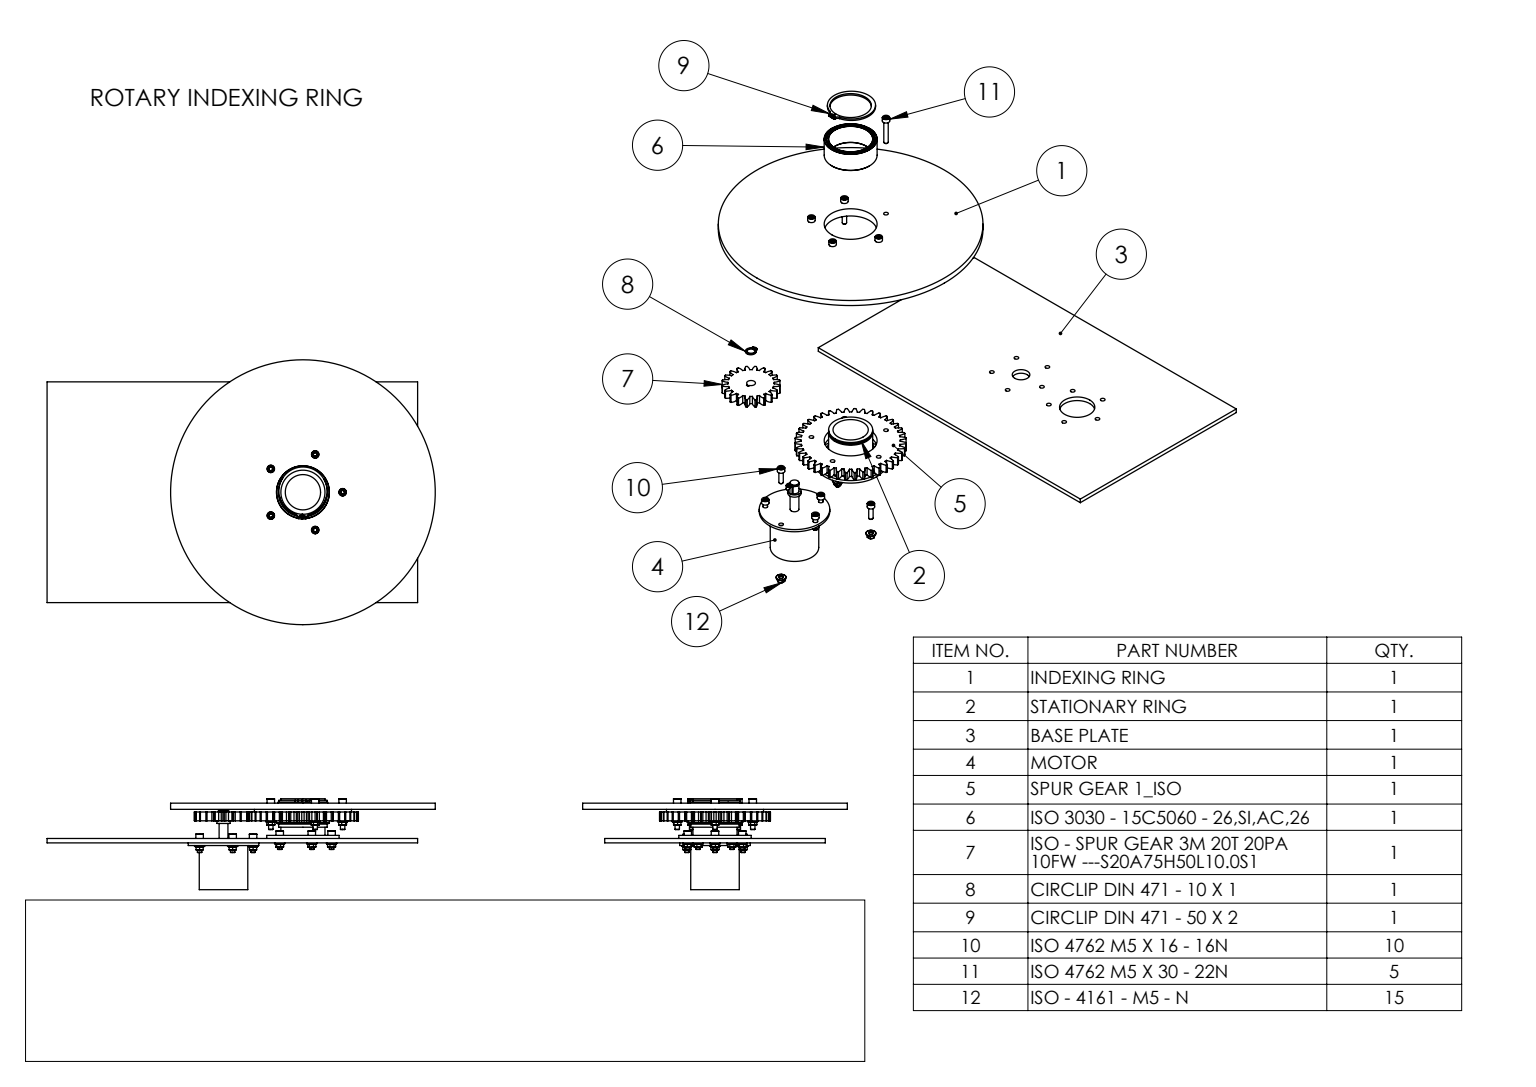
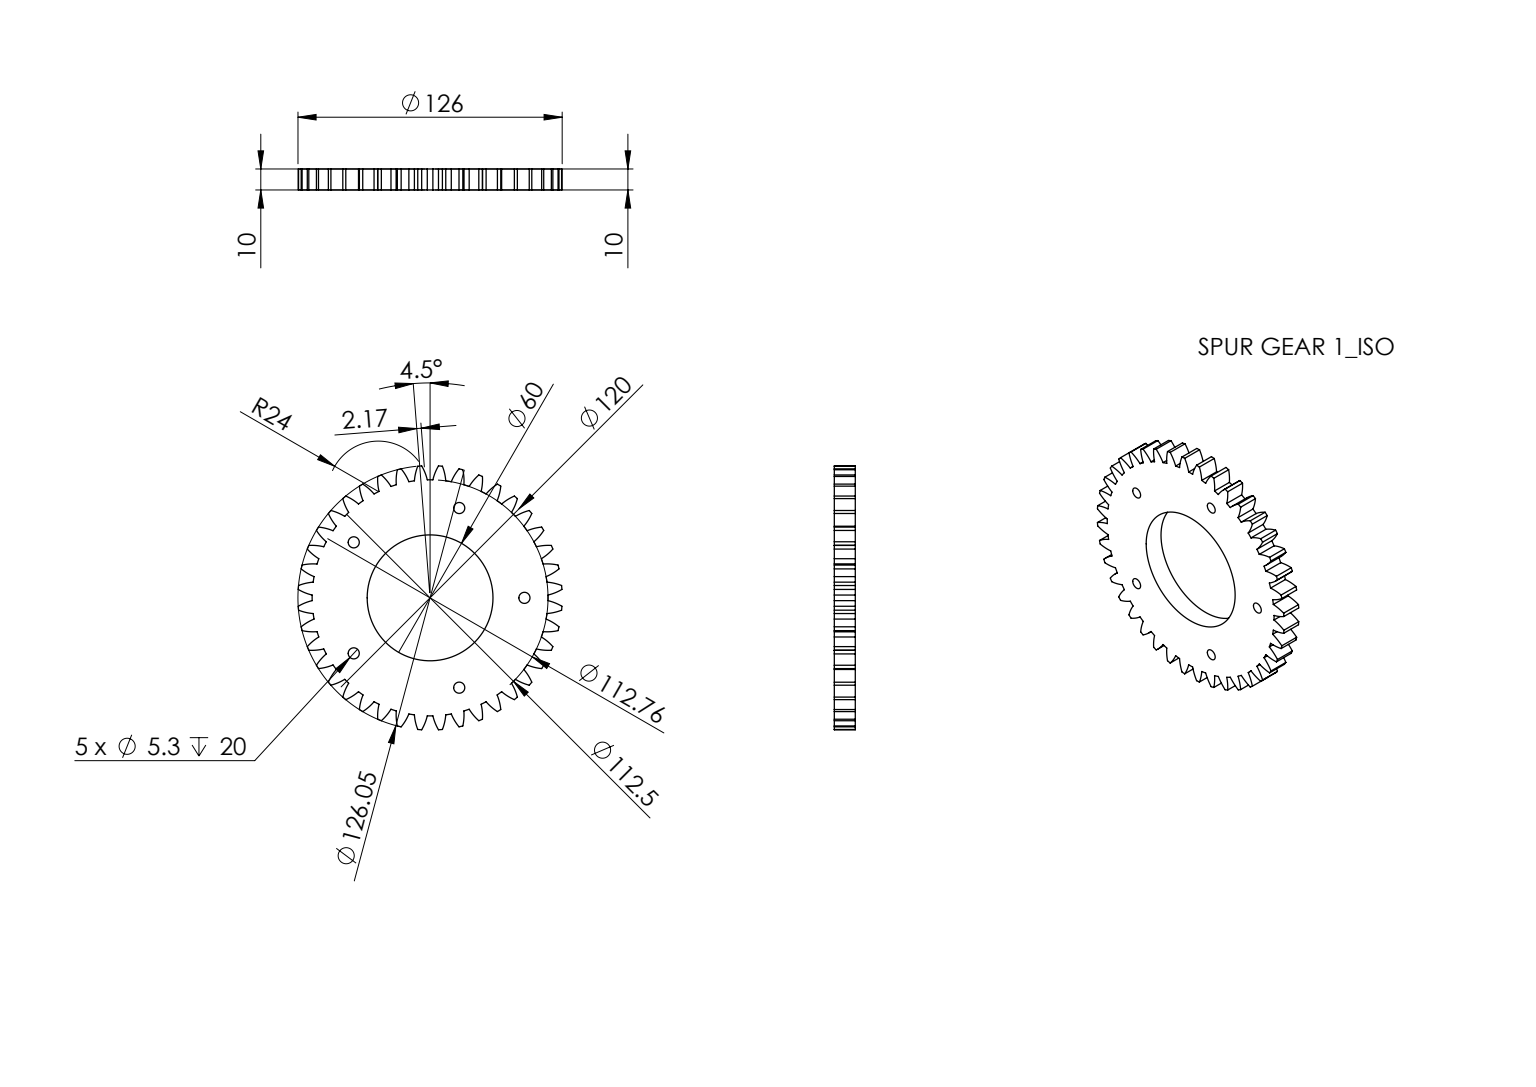
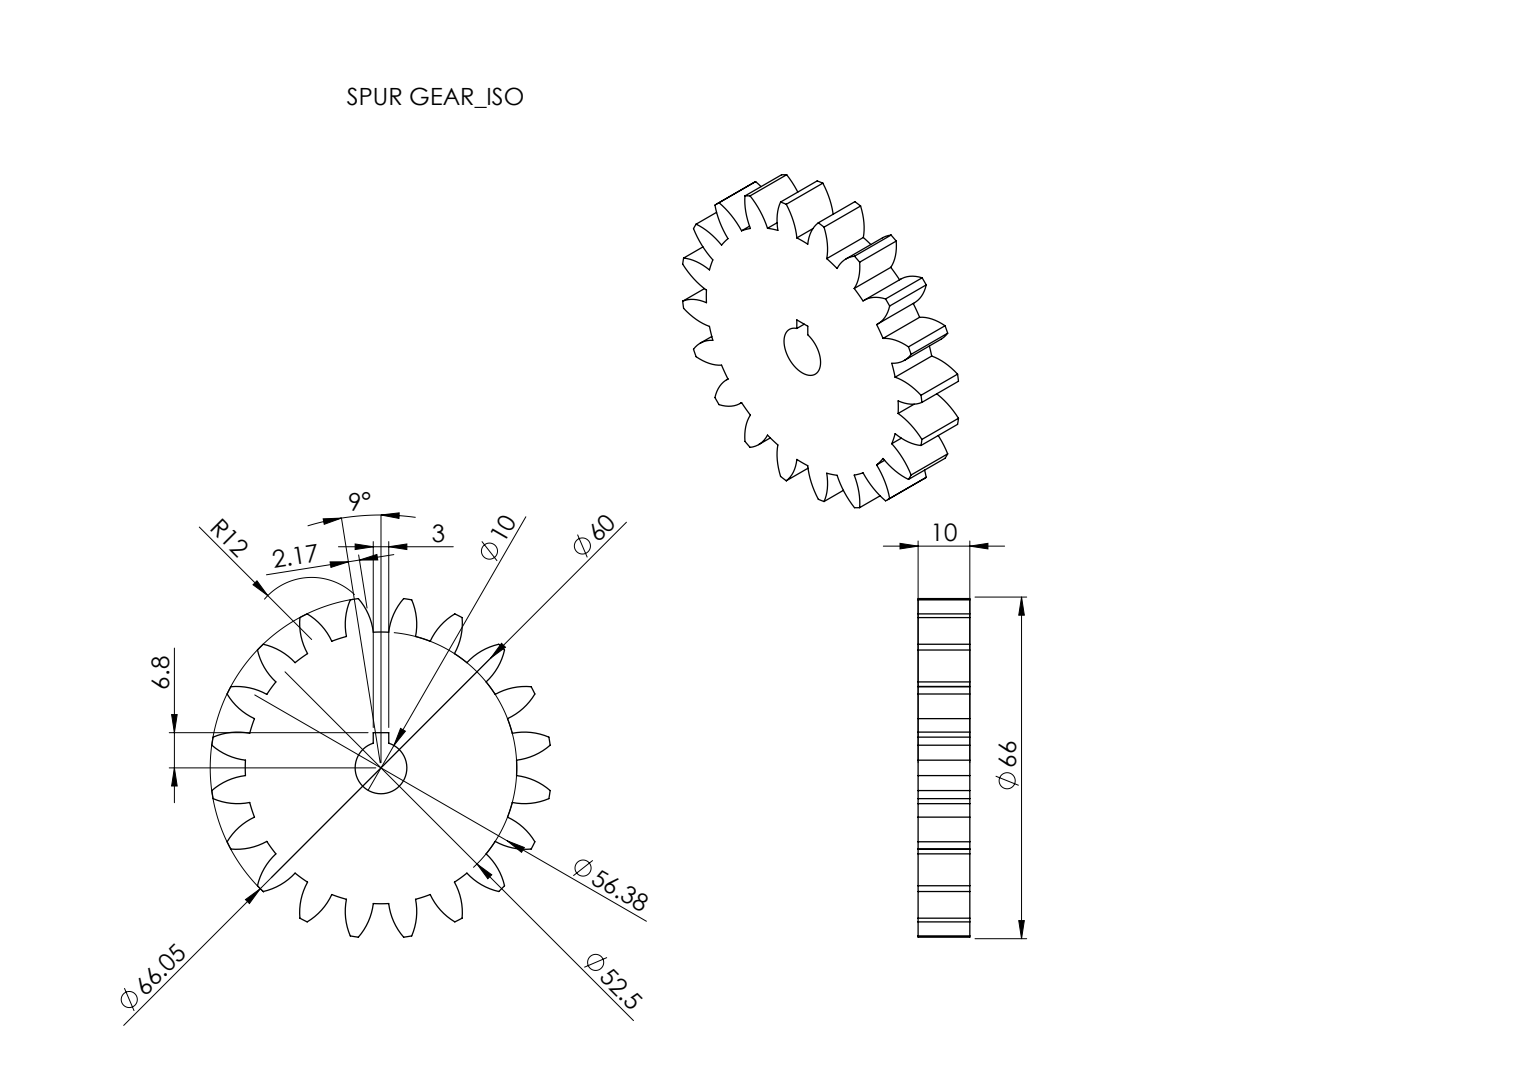
ISO-10303-21;
HEADER;
FILE_DESCRIPTION (('STEP AP214'),
    '1' );
FILE_NAME ('MAS-191',
    '2026-10-24T07:08:27',
    ( '' ),
    ( '' ),
    'SwSTEP 2.0',
    'SolidWorks 2026',
    '' );
FILE_SCHEMA (( 'AUTOMOTIVE_DESIGN' ));
ENDSEC;

DATA;
#1 = CARTESIAN_POINT ( 'NONE',  ( 0.000000000000000000, 0.000000000000000000, 0.000000000000000000 ) ) ;
#2 = VECTOR ( 'NONE', #14749, 1000.000000000000000 ) ;
#3 = EDGE_CURVE ( 'NONE', #2619, #17682, #10723, .T. ) ;
#4 = EDGE_LOOP ( 'NONE', ( #4761, #14101, #16845, #5340 ) ) ;
#5 = CIRCLE ( 'NONE', #16107, 2.649999999999999467 ) ;
#6 = VERTEX_POINT ( 'NONE', #17079 ) ;
#7 = DIRECTION ( 'NONE',  ( 0.000000000000000000, 0.000000000000000000, 1.000000000000000000 ) ) ;
#8 = CYLINDRICAL_SURFACE ( 'NONE', #267, 56.24900000005625600 ) ;
#9 = DIRECTION ( 'NONE',  ( 0.000000000000000000, 0.000000000000000000, 1.000000000000000000 ) ) ;
#10 = DIRECTION ( 'NONE',  ( -1.000000000000000000, 0.000000000000000000, 0.000000000000000000 ) ) ;
#11 = CARTESIAN_POINT ( 'NONE',  ( -79.64793068852898728, -30.00000000000000000, -31.86039329588756530 ) ) ;
#12 = EDGE_CURVE ( 'NONE', #10921, #8874, #11145, .T. ) ;
#13 = CARTESIAN_POINT ( 'NONE',  ( 0.000000000000000000, 0.000000000000000000, 0.000000000000000000 ) ) ;
#14 = DIRECTION ( 'NONE',  ( 0.000000000000000000, 0.000000000000000000, 1.000000000000000000 ) ) ;
#15 = FACE_BOUND ( 'NONE', #1592, .T. ) ;
#16 = ORIENTED_EDGE ( 'NONE', *, *, #15782, .F. ) ;
#17 = DIRECTION ( 'NONE',  ( 1.000000000000000000, 0.000000000000000000, 0.000000000000000000 ) ) ;
#18 = DIRECTION ( 'NONE',  ( 0.000000000000000000, 0.000000000000000000, 1.000000000000000000 ) ) ;
#19 = VERTEX_POINT ( 'NONE', #12878 ) ;
#20 = DIRECTION ( 'NONE',  ( 0.000000000000000000, 0.8910065241883657894, 0.4539904997395510788 ) ) ;
#21 = CIRCLE ( 'NONE', #6696, 12.00000000001200462 ) ;
#22 = CARTESIAN_POINT ( 'NONE',  ( 10.00000000000000000, 14.27431201565567065, -29.75305054077457356 ) ) ;
#23 = AXIS2_PLACEMENT_3D ( 'NONE', #13268, #7449, #2893 ) ;
#24 = VERTEX_POINT ( 'NONE', #17163 ) ;
#25 = CARTESIAN_POINT ( 'NONE',  ( 10.00000000000000000, -5.086963483077402870, 27.72801475327280585 ) ) ;
#26 = DIRECTION ( 'NONE',  ( 0.000000000000000000, 0.3090169943749410120, 0.9510565162951556406 ) ) ;
#27 = ORIENTED_EDGE ( 'NONE', *, *, #4590, .T. ) ;
#28 = CARTESIAN_POINT ( 'NONE',  ( 0.000000000000000000, -56.23315539212691050, 1.335003989221430487 ) ) ;
#29 = CARTESIAN_POINT ( 'NONE',  ( 10.00000000000000000, 24.33982105418971642, -50.71018745830419050 ) ) ;
#30 = VECTOR ( 'NONE', #9447, 1000.000000000000000 ) ;
#31 = DIRECTION ( 'NONE',  ( 0.000000000000000000, -1.000000000000000000, 0.000000000000000000 ) ) ;
#32 = CARTESIAN_POINT ( 'NONE',  ( 10.00000000000000000, 0.000000000000000000, 0.000000000000000000 ) ) ;
#33 = LINE ( 'NONE', #10310, #12031 ) ;
#34 = VERTEX_POINT ( 'NONE', #6862 ) ;
#35 = CYLINDRICAL_SURFACE ( 'NONE', #9712, 56.24900000005625600 ) ;
#36 = EDGE_LOOP ( 'NONE', ( #215, #7288, #18290, #7153 ) ) ;
#37 = CYLINDRICAL_SURFACE ( 'NONE', #14858, 56.24900000005625600 ) ;
#38 = VERTEX_POINT ( 'NONE', #8302 ) ;
#39 = ITEM_DEFINED_TRANSFORMATION ( 'NONE', 'NONE', #3191,  #8017 ) ;
#40 = ORIENTED_EDGE ( 'NONE', *, *, #3069, .F. ) ;
#41 = EDGE_CURVE ( 'NONE', #17767, #6918, #12253, .T. ) ;
#42 = EDGE_CURVE ( 'NONE', #9389, #8733, #2574, .T. ) ;
#43 = AXIS2_PLACEMENT_3D ( 'NONE', #4578, #2974, #8946 ) ;
#44 = EDGE_CURVE ( 'NONE', #931, #15024, #4657, .T. ) ;
#45 = CARTESIAN_POINT ( 'NONE',  ( 0.000000000000000000, -53.29895248911688554, 18.38754094778222026 ) ) ;
#46 = ADVANCED_FACE ( 'NONE', ( #14203 ), #12781, .T. ) ;
#47 = DIRECTION ( 'NONE',  ( 0.000000000000000000, 0.000000000000000000, 1.000000000000000000 ) ) ;
#48 = DIRECTION ( 'NONE',  ( 1.000000000000000000, 0.000000000000000000, 0.000000000000000000 ) ) ;
#49 = DIRECTION ( 'NONE',  ( 0.000000000000000000, -1.000000000000000000, 0.000000000000000000 ) ) ;
#50 = EDGE_CURVE ( 'NONE', #3645, #6188, #5249, .T. ) ;
#51 = DIRECTION ( 'NONE',  ( 0.000000000000000000, 0.000000000000000000, 1.000000000000000000 ) ) ;
#52 = CARTESIAN_POINT ( 'NONE',  ( 9.345251662538453630, -28.92794965710190525, -2.000000000000000000 ) ) ;
#53 = EDGE_CURVE ( 'NONE', #16495, #2470, #11654, .T. ) ;
#54 = ORIENTED_EDGE ( 'NONE', *, *, #7702, .F. ) ;
#55 = AXIS2_PLACEMENT_3D ( 'NONE', #9559, #12524, #9279 ) ;
#56 = CARTESIAN_POINT ( 'NONE',  ( -10.00000000000000000, 0.000000000000000000, 0.000000000000000000 ) ) ;
#57 = EDGE_CURVE ( 'NONE', #1536, #5010, #18293, .T. ) ;
#58 = CARTESIAN_POINT ( 'NONE',  ( 0.000000000000000000, 26.71881558261731016, 49.49802920186233024 ) ) ;
#59 = CARTESIAN_POINT ( 'NONE',  ( 10.00000000000000000, 42.79754323328179311, -13.90576474687299680 ) ) ;
#60 = ORIENTED_EDGE ( 'NONE', *, *, #8774, .T. ) ;
#61 = ORIENTED_EDGE ( 'NONE', *, *, #6083, .F. ) ;
#62 = PLANE ( 'NONE',  #8396 ) ;
#63 = SURFACE_STYLE_USAGE ( .BOTH. , #18719 ) ;
#64 = ORIENTED_EDGE ( 'NONE', *, *, #16565, .T. ) ;
#65 = B_SPLINE_CURVE_WITH_KNOTS ( 'NONE', 3,
 ( #1226, #12839, #18639, #3001, #8800, #7452 ),
 .UNSPECIFIED., .F., .F.,
 ( 4, 2, 4 ),
 ( 0.002365888236227977302, 0.003551327329835078910, 0.004736766423442180518 ),
 .UNSPECIFIED. ) ;
#66 = EDGE_CURVE ( 'NONE', #4445, #9928, #18675, .T. ) ;
#67 = EDGE_CURVE ( 'NONE', #3123, #6017, #15305, .T. ) ;
#68 = DIRECTION ( 'NONE',  ( 0.000000000000000000, 0.9510565162951520879, 0.3090169943749517811 ) ) ;
#69 = PLANE ( 'NONE',  #12942 ) ;
#70 = DIRECTION ( 'NONE',  ( 0.000000000000000000, 0.000000000000000000, 1.000000000000000000 ) ) ;
#71 = EDGE_CURVE ( 'NONE', #17356, #16127, #6478, .T. ) ;
#72 = VERTEX_POINT ( 'NONE', #15446 ) ;
#73 = DIRECTION ( 'NONE',  ( 1.000000000000000000, 0.000000000000000000, 0.000000000000000000 ) ) ;
#74 = VECTOR ( 'NONE', #5888, 1000.000000000000000 ) ;
#75 = ORIENTED_EDGE ( 'NONE', *, *, #4136, .T. ) ;
#76 = UNCERTAINTY_MEASURE_WITH_UNIT (LENGTH_MEASURE( 1.000000000000000082E-05 ), #4261, 'distance_accuracy_value', 'NONE');
#77 = FACE_OUTER_BOUND ( 'NONE', #12932, .T. ) ;
#78 = ORIENTED_EDGE ( 'NONE', *, *, #5790, .T. ) ;
#79 = VERTEX_POINT ( 'NONE', #8211 ) ;
#80 = DIRECTION ( 'NONE',  ( -1.000000000000000000, 0.000000000000000000, 0.000000000000000000 ) ) ;
#81 = CARTESIAN_POINT ( 'NONE',  ( 10.00000000000000000, -16.45250512421895550, 53.92768374110886498 ) ) ;
#82 = ORIENTED_EDGE ( 'NONE', *, *, #16007, .F. ) ;
#83 = ORIENTED_EDGE ( 'NONE', *, *, #2311, .T. ) ;
#84 = CARTESIAN_POINT ( 'NONE',  ( -90.00000000009001155, -38.00000000000000000, -1.301042606982603940E-15 ) ) ;
#85 =( LENGTH_UNIT ( ) NAMED_UNIT ( * ) SI_UNIT ( .MILLI., .METRE. ) );
#86 = ORIENTED_EDGE ( 'NONE', *, *, #2865, .F. ) ;
#87 = FACE_OUTER_BOUND ( 'NONE', #3507, .T. ) ;
#88 = CIRCLE ( 'NONE', #6774, 2.650000000000001243 ) ;
#89 = DIRECTION ( 'NONE',  ( 1.000000000000000000, 0.000000000000000000, 0.000000000000000000 ) ) ;
#90 = EDGE_CURVE ( 'NONE', #11121, #10536, #17145, .T. ) ;
#91 = VERTEX_POINT ( 'NONE', #6771 ) ;
#92 = PRODUCT_DEFINITION_SHAPE ( 'NONE', 'NONE',  #18847 ) ;
#93 = ORIENTED_EDGE ( 'NONE', *, *, #7771, .T. ) ;
#94 = PLANE ( 'NONE',  #12371 ) ;
#95 = CARTESIAN_POINT ( 'NONE',  ( 10.00000000000000000, 57.83923611457319680, 24.97244012287522352 ) ) ;
#96 = DIRECTION ( 'NONE',  ( 0.000000000000000000, 0.000000000000000000, 1.000000000000000000 ) ) ;
#97 = ORIENTED_EDGE ( 'NONE', *, *, #4908, .F. ) ;
#98 = FACE_OUTER_BOUND ( 'NONE', #15027, .T. ) ;
#99 = CIRCLE ( 'NONE', #8612, 2.649999999999999467 ) ;
#100 = DIRECTION ( 'NONE',  ( -1.000000000000000000, 0.000000000000000000, 0.000000000000000000 ) ) ;
#102 = CIRCLE ( 'NONE', #1309, 33.00000000003299760 ) ;
#101 = CYLINDRICAL_SURFACE ( 'NONE', #6763, 24.00000000002400213 ) ;
#103 = DIRECTION ( 'NONE',  ( -1.000000000000000000, -0.000000000000000000, 0.000000000000000000 ) ) ;
#104 = VERTEX_POINT ( 'NONE', #18489 ) ;
#105 = CLOSED_SHELL ( 'NONE', ( #14234, #17974, #624, #15916, #1588, #4692, #10387, #5528, #1896, #13092, #10492, #15607, #17035, #1733, #4595, #8031, #12836, #9009, #1125, #979, #15240, #9740, #15546, #17077, #15957, #7073, #5906 ) ) ;
#106 = CARTESIAN_POINT ( 'NONE',  ( 10.00000000000000000, 61.47135697633778761, 13.79392154159156725 ) ) ;
#107 = CARTESIAN_POINT ( 'NONE',  ( 50.00005079999999680, 0.000000000000000000, 0.000000000000000000 ) ) ;
#108 = ORIENTED_EDGE ( 'NONE', *, *, #12094, .T. ) ;
#109 = DIRECTION ( 'NONE',  ( -0.000000000000000000, 1.000000000000000000, -0.000000000000000000 ) ) ;
#110 = CYLINDRICAL_SURFACE ( 'NONE', #16518, 26.24900000002624978 ) ;
#111 = EDGE_CURVE ( 'NONE', #13893, #5833, #5452, .T. ) ;
#112 = EDGE_CURVE ( 'NONE', #16490, #11963, #8906, .T. ) ;
#113 = VECTOR ( 'NONE', #7369, 1000.000000000000000 ) ;
#114 = VERTEX_POINT ( 'NONE', #13345 ) ;
#115 = CARTESIAN_POINT ( 'NONE',  ( 0.000000000000000000, 38.81885513160045065, -40.70683587897917022 ) ) ;
#116 = CARTESIAN_POINT ( 'NONE',  ( -3.098410542199071749, -7.060458129626440815, 0.000000000000000000 ) ) ;
#117 = EDGE_LOOP ( 'NONE', ( #5102, #5293 ) ) ;
#118 = FILL_AREA_STYLE_COLOUR ( '', #4219 ) ;
#119 = DIRECTION ( 'NONE',  ( -0.000000000000000000, -0.000000000000000000, 1.000000000000000000 ) ) ;
#120 = CARTESIAN_POINT ( 'NONE',  ( -117.1020693116506379, -30.00000000000000000, -19.69080595179801207 ) ) ;
#121 = CARTESIAN_POINT ( 'NONE',  ( 0.000000000000000000, 0.000000000000000000, 3.469446951953614189E-15 ) ) ;
#122 = DIRECTION ( 'NONE',  ( 0.000000000000000000, 0.000000000000000000, 1.000000000000000000 ) ) ;
#123 = ORIENTED_EDGE ( 'NONE', *, *, #10744, .F. ) ;
#124 = DIRECTION ( 'NONE',  ( -0.000000000000000000, -0.000000000000000000, 1.000000000000000000 ) ) ;
#125 = VERTEX_POINT ( 'NONE', #12966 ) ;
#126 = COLOUR_RGB ( '',0.8941176470588234615, 0.8941176470588234615, 0.8941176470588234615 ) ;
#127 = CARTESIAN_POINT ( 'NONE',  ( -4.211140560182196957, 2.431303136016537803, -3.745885042887433514 ) ) ;
#128 = ORIENTED_EDGE ( 'NONE', *, *, #5149, .F. ) ;
#129 = ADVANCED_FACE ( 'NONE', ( #1437, #5995, #2963, #8762, #10290, #1707, #8940 ), #14754, .F. ) ;
#130 = PRODUCT_CONTEXT ( 'NONE', #17652, 'mechanical' ) ;
#131 = ORIENTED_EDGE ( 'NONE', *, *, #5631, .T. ) ;
#132 = CARTESIAN_POINT ( 'NONE',  ( 2.000000000000008882, 3.464101615137749945, 0.000000000000000000 ) ) ;
#133 = FACE_OUTER_BOUND ( 'NONE', #8514, .T. ) ;
#134 = CARTESIAN_POINT ( 'NONE',  ( 0.000000000000000000, -18.38754094778278869, 53.29895248911668659 ) ) ;
#135 = CARTESIAN_POINT ( 'NONE',  ( 13.90576474687299680, 0.000000000000000000, 42.79754323328179311 ) ) ;
#136 = CARTESIAN_POINT ( 'NONE',  ( 5.000000000000000000, -32.11449294037235802, 54.20017844242499905 ) ) ;
#137 = CARTESIAN_POINT ( 'NONE',  ( -26.29305231718568336, -30.00000000000000000, -19.10302069950552095 ) ) ;
#138 = FACE_OUTER_BOUND ( 'NONE', #567, .T. ) ;
#139 = VERTEX_POINT ( 'NONE', #10380 ) ;
#140 = ADVANCED_FACE ( 'NONE', ( #1619 ), #11545, .F. ) ;
#141 = EDGE_CURVE ( 'NONE', #9382, #18009, #4302, .T. ) ;
#142 = LINE ( 'NONE', #1937, #2927 ) ;
#143 = CARTESIAN_POINT ( 'NONE',  ( 0.000000000000000000, -34.99999999999999289, 20.00000000000000000 ) ) ;
#144 = DIRECTION ( 'NONE',  ( 0.000000000000000000, -0.5877852522924624790, -0.8090169943749551118 ) ) ;
#145 = ORIENTED_EDGE ( 'NONE', *, *, #12203, .T. ) ;
#146 = ORIENTED_EDGE ( 'NONE', *, *, #2272, .F. ) ;
#147 = CARTESIAN_POINT ( 'NONE',  ( 10.00000000000000000, -26.20671763660629594, 1.489278925039428936 ) ) ;
#148 =( GEOMETRIC_REPRESENTATION_CONTEXT ( 3 ) GLOBAL_UNCERTAINTY_ASSIGNED_CONTEXT ( ( #11684 ) ) GLOBAL_UNIT_ASSIGNED_CONTEXT ( ( #18254, #15584, #13862 ) ) REPRESENTATION_CONTEXT ( 'NONE', 'WORKASPACE' ) );
#149 = DIRECTION ( 'NONE',  ( 0.000000000000000000, 0.000000000000000000, -1.000000000000000000 ) ) ;
#150 = ORIENTED_EDGE ( 'NONE', *, *, #4149, .F. ) ;
#151 = AXIS2_PLACEMENT_3D ( 'NONE', #17609, #7507, #3331 ) ;
#152 = DIRECTION ( 'NONE',  ( -0.000000000000000000, -0.000000000000000000, -1.000000000000000000 ) ) ;
#153 = CARTESIAN_POINT ( 'NONE',  ( 0.000000000000000000, -29.75305054077482581, 14.27431201565513952 ) ) ;
#154 = EDGE_CURVE ( 'NONE', #2490, #16785, #5575, .T. ) ;
#155 = DIRECTION ( 'NONE',  ( -1.000000000000000000, 0.000000000000000000, -0.000000000000000000 ) ) ;
#156 = ORIENTED_EDGE ( 'NONE', *, *, #8629, .F. ) ;
#157 = CARTESIAN_POINT ( 'NONE',  ( 2.000000000000008882, 3.464101615137749945, 0.000000000000000000 ) ) ;
#158 = ORIENTED_EDGE ( 'NONE', *, *, #15306, .F. ) ;
#159 = FACE_OUTER_BOUND ( 'NONE', #7289, .T. ) ;
#160 = AXIS2_PLACEMENT_3D ( 'NONE', #16421, #7559, #15796 ) ;
#161 = ORIENTED_EDGE ( 'NONE', *, *, #10210, .F. ) ;
#163 = EDGE_LOOP ( 'NONE', ( #2540, #2042, #15896, #16236 ) ) ;
#162 = EDGE_CURVE ( 'NONE', #3115, #10632, #18771, .T. ) ;
#164 = ADVANCED_FACE ( 'NONE', ( #7241 ), #1349, .F. ) ;
#165 = DIRECTION ( 'NONE',  ( 0.000000000000000000, 0.000000000000000000, 1.000000000000000000 ) ) ;
#166 = CYLINDRICAL_SURFACE ( 'NONE', #15609, 30.00000000000000000 ) ;
#167 = ORIENTED_EDGE ( 'NONE', *, *, #9471, .T. ) ;
#168 = VERTEX_POINT ( 'NONE', #13239 ) ;
#169 = CARTESIAN_POINT ( 'NONE',  ( 10.00000000000000000, 10.11537145609457156, -55.33199130079773909 ) ) ;
#170 = ADVANCED_FACE ( 'NONE', ( #11899 ), #15915, .T. ) ;
#171 = ORIENTED_EDGE ( 'NONE', *, *, #3220, .F. ) ;
#172 = DIRECTION ( 'NONE',  ( -1.000000000000000000, 0.000000000000000000, 0.000000000000000000 ) ) ;
#173 = AXIS2_PLACEMENT_3D ( 'NONE', #16539, #10357, #10634 ) ;
#174 = EDGE_CURVE ( 'NONE', #11247, #17285, #17354, .T. ) ;
#175 = CIRCLE ( 'NONE', #12635, 2.649999999999999467 ) ;
#176 = AXIS2_PLACEMENT_3D ( 'NONE', #3253, #211, #16295 ) ;
#177 = EDGE_CURVE ( 'NONE', #2698, #7707, #13480, .T. ) ;
#178 = CARTESIAN_POINT ( 'NONE',  ( 0.000000000000000000, 6.799999999999999822, 1.500000000000000000 ) ) ;
#179 = VERTEX_POINT ( 'NONE', #8579 ) ;
#180 = VECTOR ( 'NONE', #16052, 1000.000000000000000 ) ;
#181 = ORIENTED_EDGE ( 'NONE', *, *, #5658, .T. ) ;
#182 = DIRECTION ( 'NONE',  ( 0.000000000000000000, 0.9876883405951371042, 0.1564344650402347547 ) ) ;
#183 = DIRECTION ( 'NONE',  ( -0.000000000000000000, 1.000000000000000000, 1.224646799147353207E-16 ) ) ;
#185 = AXIS2_PLACEMENT_3D ( 'NONE', #9363, #1260, #1164 ) ;
#184 = CARTESIAN_POINT ( 'NONE',  ( 10.00000000000000000, -14.19907017806852245, -22.07705612348854984 ) ) ;
#186 = VERTEX_POINT ( 'NONE', #14473 ) ;
#187 = CARTESIAN_POINT ( 'NONE',  ( -4.211399284164270895, 2.459729995988205964, -3.751162237960538715 ) ) ;
#188 = CARTESIAN_POINT ( 'NONE',  ( 10.00000000000000000, -53.89344778774800915, -16.10733642026540480 ) ) ;
#189 = FACE_OUTER_BOUND ( 'NONE', #10900, .T. ) ;
#190 = AXIS2_PLACEMENT_3D ( 'NONE', #10322, #1927, #7639 ) ;
#191 = DIRECTION ( 'NONE',  ( 0.000000000000000000, 0.000000000000000000, 1.000000000000000000 ) ) ;
#192 = VERTEX_POINT ( 'NONE', #13063 ) ;
#193 = LINE ( 'NONE', #5991, #9405 ) ;
#194 = AXIS2_PLACEMENT_3D ( 'NONE', #3141, #10184, #17431 ) ;
#195 = VERTEX_POINT ( 'NONE', #22 ) ;
#196 = CARTESIAN_POINT ( 'NONE',  ( 10.00000000000000178, 6.799999999999999822, 1.500000000000000000 ) ) ;
#197 = DIRECTION ( 'NONE',  ( 0.000000000000000000, 0.000000000000000000, 1.000000000000000000 ) ) ;
#198 = EDGE_CURVE ( 'NONE', #10779, #13712, #7678, .T. ) ;
#199 = MECHANICAL_DESIGN_GEOMETRIC_PRESENTATION_REPRESENTATION (  '', ( #3240 ), #15710 ) ;
#200 = CIRCLE ( 'NONE', #7785, 30.00000000000000711 ) ;
#201 = AXIS2_PLACEMENT_3D ( 'NONE', #1014, #18051, #5099 ) ;
#202 = VERTEX_POINT ( 'NONE', #4387 ) ;
#203 = CARTESIAN_POINT ( 'NONE',  ( 10.00000000000000000, 0.000000000000000000, 0.000000000000000000 ) ) ;
#204 = CYLINDRICAL_SURFACE ( 'NONE', #43, 55.00000000000000000 ) ;
#205 = VERTEX_POINT ( 'NONE', #10192 ) ;
#206 = CARTESIAN_POINT ( 'NONE',  ( 10.00000000000000000, 13.79392154159134165, 61.47135697633784446 ) ) ;
#207 = DIRECTION ( 'NONE',  ( 0.000000000000000000, 0.000000000000000000, 1.000000000000000000 ) ) ;
#208 = DIRECTION ( 'NONE',  ( 0.000000000000000000, 0.000000000000000000, -1.000000000000000000 ) ) ;
#209 = CARTESIAN_POINT ( 'NONE',  ( 0.000000000000000000, -26.45033635316118747, 33.75576474687270689 ) ) ;
#210 = AXIS2_PLACEMENT_3D ( 'NONE', #17149, #4374, #9896 ) ;
#211 = DIRECTION ( 'NONE',  ( 0.000000000000000000, 0.000000000000000000, 1.000000000000000000 ) ) ;
#212 = ORIENTED_EDGE ( 'NONE', *, *, #1109, .T. ) ;
#213 = CARTESIAN_POINT ( 'NONE',  ( 5.021051876504148963E-15, -26.50000000000000000, 41.00000000000000000 ) ) ;
#214 = CIRCLE ( 'NONE', #13847, 12.00000000001200462 ) ;
#215 = ORIENTED_EDGE ( 'NONE', *, *, #7148, .F. ) ;
#216 = VECTOR ( 'NONE', #7709, 1000.000000000000000 ) ;
#217 = CARTESIAN_POINT ( 'NONE',  ( -2.354826896168714434, -6.962563485461402024, 0.000000000000000000 ) ) ;
#218 = ORIENTED_EDGE ( 'NONE', *, *, #8699, .T. ) ;
#219 = VECTOR ( 'NONE', #13244, 1000.000000000000000 ) ;
#220 = EDGE_CURVE ( 'NONE', #7351, #4921, #14999, .T. ) ;
#221 = PRODUCT_CONTEXT ( 'NONE', #9864, 'mechanical' ) ;
#222 = ORIENTED_EDGE ( 'NONE', *, *, #3085, .T. ) ;
#223 = AXIS2_PLACEMENT_3D ( 'NONE', #7888, #16549, #14847 ) ;
#224 = CARTESIAN_POINT ( 'NONE',  ( 2.500000000000000000, 0.000000000000000000, 0.000000000000000000 ) ) ;
#225 = CARTESIAN_POINT ( 'NONE',  ( 10.00000000000000000, -39.14194549634336084, -40.58063702438384013 ) ) ;
#226 = CIRCLE ( 'NONE', #3261, 2.649999999999992806 ) ;
#227 = DIRECTION ( 'NONE',  ( -0.000000000000000000, 1.000000000000000000, -0.000000000000000000 ) ) ;
#228 = ADVANCED_FACE ( 'NONE', ( #13154 ), #110, .T. ) ;
#229 = CARTESIAN_POINT ( 'NONE',  ( 0.000000000000000000, 26.45033635316149301, 36.40576474687247099 ) ) ;
#230 = CARTESIAN_POINT ( 'NONE',  ( 2.499999999999999556, 0.000000000000000000, 3.469446951953614189E-15 ) ) ;
#231 = DIRECTION ( 'NONE',  ( -1.000000000000000000, 0.000000000000000000, -0.000000000000000000 ) ) ;
#232 = DIRECTION ( 'NONE',  ( -1.000000000000000000, -0.000000000000000000, -0.000000000000000000 ) ) ;
#233 = CARTESIAN_POINT ( 'NONE',  ( -10.00000000000000000, 0.000000000000000000, 0.000000000000000000 ) ) ;
#234 = ORIENTED_EDGE ( 'NONE', *, *, #4136, .F. ) ;
#235 = EDGE_CURVE ( 'NONE', #17488, #2222, #5868, .T. ) ;
#236 = CARTESIAN_POINT ( 'NONE',  ( 10.00000000000000000, 0.000000000000000000, 0.000000000000000000 ) ) ;
#237 = CARTESIAN_POINT ( 'NONE',  ( 10.00000000000000000, -55.51919907100644735, -9.823366686501268319 ) ) ;
#238 = ORIENTED_EDGE ( 'NONE', *, *, #16129, .T. ) ;
#239 = ORIENTED_EDGE ( 'NONE', *, *, #9480, .F. ) ;
#240 = CARTESIAN_POINT ( 'NONE',  ( -90.00000000009001155, -38.00000000000000000, -1.301042606982603940E-15 ) ) ;
#241 = DIRECTION ( 'NONE',  ( 1.000000000000000000, 0.000000000000000000, 0.000000000000000000 ) ) ;
#242 = CARTESIAN_POINT ( 'NONE',  ( 10.04305231718605285, -30.00000000000000000, -30.90933677959240811 ) ) ;
#243 = VERTEX_POINT ( 'NONE', #16663 ) ;
#244 = AXIS2_PLACEMENT_3D ( 'NONE', #7174, #48, #4147 ) ;
#245 = VECTOR ( 'NONE', #14490, 1000.000000000000000 ) ;
#246 = DIRECTION ( 'NONE',  ( 0.000000000000000000, 0.000000000000000000, 1.000000000000000000 ) ) ;
#247 = LINE ( 'NONE', #16244, #12318 ) ;
#248 = AXIS2_PLACEMENT_3D ( 'NONE', #8151, #16908, #9666 ) ;
#249 = DIRECTION ( 'NONE',  ( 0.000000000000000000, 0.000000000000000000, 1.000000000000000000 ) ) ;
#250 = ORIENTED_EDGE ( 'NONE', *, *, #2735, .T. ) ;
#251 = CARTESIAN_POINT ( 'NONE',  ( 2.000000000000005329, -3.464101615137751722, 0.000000000000000000 ) ) ;
#252 = AXIS2_PLACEMENT_3D ( 'NONE', #13073, #8403, #2977 ) ;
#253 = ORIENTED_EDGE ( 'NONE', *, *, #16333, .F. ) ;
#254 = UNCERTAINTY_MEASURE_WITH_UNIT (LENGTH_MEASURE( 1.000000000000000082E-05 ), #934, 'distance_accuracy_value', 'NONE');
#255 = LINE ( 'NONE', #14921, #9366 ) ;
#256 = EDGE_LOOP ( 'NONE', ( #13526, #15822 ) ) ;
#257 = DIRECTION ( 'NONE',  ( -0.000000000000000000, -1.000000000000000000, -0.000000000000000000 ) ) ;
#258 = LINE ( 'NONE', #11691, #3125 ) ;
#259 = ORIENTED_EDGE ( 'NONE', *, *, #7474, .F. ) ;
#260 = EDGE_LOOP ( 'NONE', ( #2275, #5980, #9068 ) ) ;
#261 = DIRECTION ( 'NONE',  ( 0.000000000000000000, -0.1564344650402171299, -0.9876883405951399908 ) ) ;
#262 = VERTEX_POINT ( 'NONE', #3626 ) ;
#263 = FACE_OUTER_BOUND ( 'NONE', #4095, .T. ) ;
#264 = AXIS2_PLACEMENT_3D ( 'NONE', #7455, #9080, #11756 ) ;
#265 = CIRCLE ( 'NONE', #10902, 23.50000000000000355 ) ;
#266 = CIRCLE ( 'NONE', #8445, 2.500000000000000444 ) ;
#267 = AXIS2_PLACEMENT_3D ( 'NONE', #15816, #9999, #2765 ) ;
#268 = VECTOR ( 'NONE', #16945, 1000.000000000000000 ) ;
#269 = ADVANCED_FACE ( 'NONE', ( #12188 ), #18082, .T. ) ;
#270 = EDGE_CURVE ( 'NONE', #10074, #2470, #10746, .T. ) ;
#271 = DIRECTION ( 'NONE',  ( -1.000000000000000000, -0.000000000000000000, 0.000000000000000000 ) ) ;
#272 = EDGE_CURVE ( 'NONE', #1366, #4272, #1923, .T. ) ;
#273 = ORIENTED_EDGE ( 'NONE', *, *, #14374, .F. ) ;
#274 = EDGE_CURVE ( 'NONE', #652, #912, #17441, .T. ) ;
#275 = CIRCLE ( 'NONE', #6366, 63.00000000006298961 ) ;
#276 = VERTEX_POINT ( 'NONE', #6560 ) ;
#277 = CARTESIAN_POINT ( 'NONE',  ( -90.67999921423555065, 1.000000000000018208, -4.751589320297106234 ) ) ;
#278 = DIRECTION ( 'NONE',  ( 1.000000000000000000, 0.000000000000000000, 0.000000000000000000 ) ) ;
#279 = CARTESIAN_POINT ( 'NONE',  ( 10.00000000000000000, 22.07705612348859958, -14.19907017806844252 ) ) ;
#280 = VERTEX_POINT ( 'NONE', #17994 ) ;
#281 = CARTESIAN_POINT ( 'NONE',  ( -4.197477534772231955, 0.8522413273724368521, -3.505042416683225692 ) ) ;
#282 = AXIS2_PLACEMENT_3D ( 'NONE', #13219, #16170, #3319 ) ;
#283 = EDGE_CURVE ( 'NONE', #12652, #8705, #12569, .T. ) ;
#284 = FACE_OUTER_BOUND ( 'NONE', #13491, .T. ) ;
#285 = CARTESIAN_POINT ( 'NONE',  ( 0.000000000000000000, -22.76987570971509811, -23.88582760061506249 ) ) ;
#286 = DIRECTION ( 'NONE',  ( -0.000000000000000000, -1.000000000000000000, -0.000000000000000000 ) ) ;
#287 = ORIENTED_EDGE ( 'NONE', *, *, #9710, .T. ) ;
#288 = DIRECTION ( 'NONE',  ( 0.000000000000000000, 0.000000000000000000, 1.000000000000000000 ) ) ;
#289 = CARTESIAN_POINT ( 'NONE',  ( 10.00000000000000000, 25.38428207620322752, 6.681932690257054830 ) ) ;
#291 = EDGE_CURVE ( 'NONE', #7622, #9920, #13522, .T. ) ;
#290 = ORIENTED_EDGE ( 'NONE', *, *, #8143, .F. ) ;
#292 = DIRECTION ( 'NONE',  ( 0.000000000000000000, -0.3090169943749348502, -0.9510565162951576390 ) ) ;
#293 = CARTESIAN_POINT ( 'NONE',  ( 0.000000000000000000, 0.000000000000000000, 0.000000000000000000 ) ) ;
#294 = CIRCLE ( 'NONE', #10631, 2.649999999999999467 ) ;
#295 = EDGE_CURVE ( 'NONE', #2351, #16747, #1024, .T. ) ;
#296 = AXIS2_PLACEMENT_3D ( 'NONE', #5203, #15025, #16454 ) ;
#297 = AXIS2_PLACEMENT_3D ( 'NONE', #16898, #13842, #16521 ) ;
#298 = VERTEX_POINT ( 'NONE', #12276 ) ;
#299 = CARTESIAN_POINT ( 'NONE',  ( 0.5000000000000000000, -6.429618962271402616, -1.000000000000000000 ) ) ;
#300 = CARTESIAN_POINT ( 'NONE',  ( -23.48826165280196321, 13.24999999999999467, -0.7426739052322690604 ) ) ;
#301 = ORIENTED_EDGE ( 'NONE', *, *, #12426, .F. ) ;
#302 = CARTESIAN_POINT ( 'NONE',  ( -1.149515148933662080E-15, -4.736529461166056443, -3.681130640444383317 ) ) ;
#303 = EDGE_CURVE ( 'NONE', #6749, #12292, #6178, .T. ) ;
#304 = DIRECTION ( 'NONE',  ( -1.000000000000000000, 0.000000000000000000, -0.000000000000000000 ) ) ;
#305 = EDGE_CURVE ( 'NONE', #13142, #9008, #11661, .T. ) ;
#306 = LINE ( 'NONE', #5042, #9675 ) ;
#307 = CIRCLE ( 'NONE', #11570, 12.00000000001200640 ) ;
#308 = DIRECTION ( 'NONE',  ( 1.000000000000000000, 0.000000000000000000, 0.000000000000000000 ) ) ;
#309 = CYLINDRICAL_SURFACE ( 'NONE', #6869, 26.24900000002624978 ) ;
#310 = EDGE_LOOP ( 'NONE', ( #17511, #1241, #2457, #12125 ) ) ;
#311 = CARTESIAN_POINT ( 'NONE',  ( 10.00000000000000000, 33.95787273855309252, -45.00825343884985585 ) ) ;
#312 = ORIENTED_EDGE ( 'NONE', *, *, #6097, .T. ) ;
#313 = CARTESIAN_POINT ( 'NONE',  ( 10.00000000000000000, -46.20417134726108088, -32.31183295104820985 ) ) ;
#314 = ORIENTED_EDGE ( 'NONE', *, *, #13333, .F. ) ;
#315 = CONTEXT_DEPENDENT_SHAPE_REPRESENTATION ( #13286, #6015 ) ;
#316 = ORIENTED_EDGE ( 'NONE', *, *, #16930, .F. ) ;
#317 = ORIENTED_EDGE ( 'NONE', *, *, #10109, .T. ) ;
#318 = AXIS2_PLACEMENT_3D ( 'NONE', #9764, #18617, #15573 ) ;
#319 = ORIENTED_EDGE ( 'NONE', *, *, #6313, .F. ) ;
#320 = VECTOR ( 'NONE', #10301, 1000.000000000000000 ) ;
#321 = DIRECTION ( 'NONE',  ( -1.000000000000000000, 0.000000000000000000, -0.000000000000000000 ) ) ;
#322 = CARTESIAN_POINT ( 'NONE',  ( 10.00000000000000000, 3.730438010304726770, -27.94286728106388296 ) ) ;
#323 = DIRECTION ( 'NONE',  ( -1.000000000000000000, 0.000000000000000000, 0.000000000000000000 ) ) ;
#324 = ADVANCED_FACE ( 'NONE', ( #3519 ), #10462, .T. ) ;
#325 = CYLINDRICAL_SURFACE ( 'NONE', #2758, 56.24900000005625600 ) ;
#326 = LINE ( 'NONE', #14699, #2052 ) ;
#327 = DIRECTION ( 'NONE',  ( 1.000000000000000000, 0.000000000000000000, 0.000000000000000000 ) ) ;
#328 = CARTESIAN_POINT ( 'NONE',  ( -4.000000000000000000, -2.309401076758512694, -3.433295621305382461 ) ) ;
#329 = CARTESIAN_POINT ( 'NONE',  ( 0.000000000000000000, 0.000000000000000000, -2.000000000000000000 ) ) ;
#330 = ORIENTED_EDGE ( 'NONE', *, *, #18226, .F. ) ;
#331 = DIRECTION ( 'NONE',  ( 0.000000000000000000, 0.000000000000000000, 1.000000000000000000 ) ) ;
#332 = CARTESIAN_POINT ( 'NONE',  ( 10.00000000000000000, 0.000000000000000000, 0.000000000000000000 ) ) ;
#333 = DIRECTION ( 'NONE',  ( 0.000000000000000000, 1.000000000000000000, 0.000000000000000000 ) ) ;
#334 = EDGE_LOOP ( 'NONE', ( #9936, #9386, #7839, #1385 ) ) ;
#335 = EDGE_LOOP ( 'NONE', ( #6320, #13765, #5503, #3259, #11558 ) ) ;
#336 = CYLINDRICAL_SURFACE ( 'NONE', #2323, 63.00000000006298961 ) ;
#337 = VECTOR ( 'NONE', #1446, 1000.000000000000114 ) ;
#338 = CARTESIAN_POINT ( 'NONE',  ( 10.04305231718579705, -21.50000000000000000, 30.90933677959249337 ) ) ;
#339 = CARTESIAN_POINT ( 'NONE',  ( 10.00000000000000000, 39.14194549634364506, 40.58063702438359144 ) ) ;
#340 = ORIENTED_EDGE ( 'NONE', *, *, #305, .F. ) ;
#341 = EDGE_CURVE ( 'NONE', #9120, #6839, #4855, .T. ) ;
#342 = EDGE_CURVE ( 'NONE', #3837, #6567, #9219, .T. ) ;
#343 = DIRECTION ( 'NONE',  ( 0.000000000000000000, 0.000000000000000000, -1.000000000000000000 ) ) ;
#344 = DIRECTION ( 'NONE',  ( 0.000000000000000000, 0.000000000000000000, 1.000000000000000000 ) ) ;
#345 = FACE_OUTER_BOUND ( 'NONE', #959, .T. ) ;
#346 = EDGE_LOOP ( 'NONE', ( #14600, #18802, #11785, #7106 ) ) ;
#347 = DIRECTION ( 'NONE',  ( -1.000000000000000000, -0.000000000000000000, 0.000000000000000000 ) ) ;
#348 = EDGE_LOOP ( 'NONE', ( #7542, #2578 ) ) ;
#349 = CARTESIAN_POINT ( 'NONE',  ( 5.200000000000002842, 0.000000000000000000, 2.500000000000000444 ) ) ;
#350 = ORIENTED_EDGE ( 'NONE', *, *, #9102, .F. ) ;
#351 = DIRECTION ( 'NONE',  ( 0.000000000000000000, 0.000000000000000000, 1.000000000000000000 ) ) ;
#352 = CARTESIAN_POINT ( 'NONE',  ( -1.360585162435467455, 4.061296242128285883, -3.505054077164959203 ) ) ;
#353 = VERTEX_POINT ( 'NONE', #13434 ) ;
#354 = EDGE_LOOP ( 'NONE', ( #10863, #11832 ) ) ;
#355 = CARTESIAN_POINT ( 'NONE',  ( -27.29487558977753991, 1.305124410222464393, -2.000000000000000000 ) ) ;
#356 = EDGE_LOOP ( 'NONE', ( #2421, #4949, #7612, #4912 ) ) ;
#357 = CYLINDRICAL_SURFACE ( 'NONE', #5137, 56.24900000005625600 ) ;
#358 = CARTESIAN_POINT ( 'NONE',  ( -4.000000000000000000, 2.309401076758498483, -3.433295621305379353 ) ) ;
#359 = ORIENTED_EDGE ( 'NONE', *, *, #90, .T. ) ;
#360 = ORIENTED_EDGE ( 'NONE', *, *, #3516, .T. ) ;
#361 = DIRECTION ( 'NONE',  ( 0.000000000000000000, 0.000000000000000000, 1.000000000000000000 ) ) ;
#362 = LINE ( 'NONE', #1882, #10479 ) ;
#363 = DIRECTION ( 'NONE',  ( 0.000000000000000000, -0.5877852522924801315, 0.8090169943749422332 ) ) ;
#364 = VERTEX_POINT ( 'NONE', #13623 ) ;
#365 = DIRECTION ( 'NONE',  ( 2.220446049250313081E-16, 0.000000000000000000, 1.000000000000000000 ) ) ;
#366 = VECTOR ( 'NONE', #1757, 1000.000000000000000 ) ;
#367 = DIRECTION ( 'NONE',  ( -0.9998647328874151752, -0.01644736842105263067, 0.000000000000000000 ) ) ;
#368 = DIRECTION ( 'NONE',  ( 0.000000000000000000, -0.000000000000000000, -1.000000000000000000 ) ) ;
#369 = DIRECTION ( 'NONE',  ( -1.000000000000000000, -0.000000000000000000, -0.000000000000000000 ) ) ;
#370 = ORIENTED_EDGE ( 'NONE', *, *, #11687, .F. ) ;
#371 = DIRECTION ( 'NONE',  ( 0.000000000000000000, 0.8090169943749444537, 0.5877852522924770229 ) ) ;
#372 = EDGE_CURVE ( 'NONE', #3496, #11369, #16387, .T. ) ;
#373 = DIRECTION ( 'NONE',  ( 0.000000000000000000, 0.000000000000000000, 1.000000000000000000 ) ) ;
#374 = AXIS2_PLACEMENT_3D ( 'NONE', #16083, #3127, #12944 ) ;
#375 = EDGE_CURVE ( 'NONE', #12355, #6629, #15146, .T. ) ;
#376 = EDGE_LOOP ( 'NONE', ( #4569, #16538, #11504, #3822 ) ) ;
#377 = DIRECTION ( 'NONE',  ( 0.000000000000000000, 0.3090169943749479509, -0.9510565162951533091 ) ) ;
#378 = DIRECTION ( 'NONE',  ( 1.000000000000000000, 0.000000000000000000, 0.000000000000000000 ) ) ;
#379 = EDGE_CURVE ( 'NONE', #3115, #12051, #15919, .T. ) ;
#380 = VERTEX_POINT ( 'NONE', #571 ) ;
#381 = AXIS2_PLACEMENT_3D ( 'NONE', #3992, #9793, #15604 ) ;
#382 = CARTESIAN_POINT ( 'NONE',  ( 10.00000000000000000, 32.46095361140700675, -5.940243314903877803 ) ) ;
#383 = EDGE_CURVE ( 'NONE', #6075, #13137, #5526, .T. ) ;
#384 = CIRCLE ( 'NONE', #18634, 24.00000000002399503 ) ;
#385 = ORIENTED_EDGE ( 'NONE', *, *, #14014, .F. ) ;
#386 = VECTOR ( 'NONE', #8852, 1000.000000000000000 ) ;
#387 = CARTESIAN_POINT ( 'NONE',  ( -6.473970235329672780E-16, -4.862606272033106691, -3.745885042887442395 ) ) ;
#388 = CARTESIAN_POINT ( 'NONE',  ( -11.15000000000000391, 3.673940397442059967E-15, -30.00000000000000711 ) ) ;
#389 = CARTESIAN_POINT ( 'NONE',  ( 10.04305231718605285, -26.50000000000000000, -30.90933677959240811 ) ) ;
#390 = DIRECTION ( 'NONE',  ( 0.000000000000000000, -1.000000000000000000, 0.000000000000000000 ) ) ;
#391 = DIRECTION ( 'NONE',  ( 1.000000000000000000, 0.000000000000000000, 0.000000000000000000 ) ) ;
#392 = ORIENTED_EDGE ( 'NONE', *, *, #3, .F. ) ;
#393 = DIRECTION ( 'NONE',  ( 0.000000000000000000, 0.000000000000000000, 1.000000000000000000 ) ) ;
#394 = ORIENTED_EDGE ( 'NONE', *, *, #4067, .T. ) ;
#395 = EDGE_CURVE ( 'NONE', #2599, #6420, #1243, .T. ) ;
#396 = EDGE_CURVE ( 'NONE', #5722, #407, #9783, .T. ) ;
#397 = PRODUCT_DEFINITION_SHAPE ( 'NONE', 'NONE',  #18819 ) ;
#398 = FILL_AREA_STYLE_COLOUR ( '', #126 ) ;
#399 = DIRECTION ( 'NONE',  ( -1.000000000000000000, 0.000000000000000000, 0.000000000000000000 ) ) ;
#400 = ORIENTED_EDGE ( 'NONE', *, *, #15230, .T. ) ;
#401 = ITEM_DEFINED_TRANSFORMATION ( 'NONE', 'NONE', #18387,  #8017 ) ;
#402 = EDGE_CURVE ( 'NONE', #11928, #9088, #2271, .T. ) ;
#403 = ORIENTED_EDGE ( 'NONE', *, *, #7543, .T. ) ;
#404 = AXIS2_PLACEMENT_3D ( 'NONE', #6381, #13801, #4663 ) ;
#405 = EDGE_CURVE ( 'NONE', #10887, #2703, #6947, .T. ) ;
#406 = EDGE_LOOP ( 'NONE', ( #5497, #14541, #4371, #16219 ) ) ;
#407 = VERTEX_POINT ( 'NONE', #17057 ) ;
#408 = CARTESIAN_POINT ( 'NONE',  ( 10.00000000000000000, -27.94286728106395756, 3.730438010304225394 ) ) ;
#409 = CYLINDRICAL_SURFACE ( 'NONE', #7915, 2.649999999999995914 ) ;
#410 = CARTESIAN_POINT ( 'NONE',  ( -31.74999999999995737, 0.000000000000000000, 0.000000000000000000 ) ) ;
#411 = DIRECTION ( 'NONE',  ( 0.000000000000000000, 0.000000000000000000, -1.000000000000000000 ) ) ;
#412 = AXIS2_PLACEMENT_3D ( 'NONE', #11583, #15864, #4156 ) ;
#413 = CARTESIAN_POINT ( 'NONE',  ( 0.000000000000000000, 3.000000000000000000, 0.000000000000000000 ) ) ;
#414 = DIRECTION ( 'NONE',  ( -1.000000000000000000, -0.000000000000000000, -0.000000000000000000 ) ) ;
#415 = CARTESIAN_POINT ( 'NONE',  ( -4.000000000000000888, -1.539600717839011201, -3.300726591567081591 ) ) ;
#416 = CARTESIAN_POINT ( 'NONE',  ( 4.249769933734876659, -30.10148593525447680, -2.000000000000000000 ) ) ;
#417 = VERTEX_POINT ( 'NONE', #3999 ) ;
#418 = DIRECTION ( 'NONE',  ( 0.000000000000000000, 0.000000000000000000, 1.000000000000000000 ) ) ;
#419 = DIRECTION ( 'NONE',  ( -1.000000000000000000, 0.000000000000000000, -0.000000000000000000 ) ) ;
#420 = CARTESIAN_POINT ( 'NONE',  ( 32.50000000000000000, -30.00000000000000000, 3.680389326632394941E-13 ) ) ;
#421 = VERTEX_POINT ( 'NONE', #1046 ) ;
#422 = ORIENTED_EDGE ( 'NONE', *, *, #16105, .T. ) ;
#423 = DIRECTION ( 'NONE',  ( 0.000000000000000000, 0.000000000000000000, 1.000000000000000000 ) ) ;
#424 = DIRECTION ( 'NONE',  ( 0.000000000000000000, 0.000000000000000000, 1.000000000000000000 ) ) ;
#425 = DIRECTION ( 'NONE',  ( 0.000000000000000000, 1.000000000000000000, 0.000000000000000000 ) ) ;
#426 = ORIENTED_EDGE ( 'NONE', *, *, #405, .T. ) ;
#427 = EDGE_CURVE ( 'NONE', #12688, #15321, #15425, .T. ) ;
#428 = VECTOR ( 'NONE', #12992, 1000.000000000000000 ) ;
#429 = DIRECTION ( 'NONE',  ( 1.000000000000000000, 0.000000000000000000, 0.000000000000000000 ) ) ;
#430 = DIRECTION ( 'NONE',  ( 1.000000000000000000, 0.000000000000000000, 0.000000000000000000 ) ) ;
#431 = DIRECTION ( 'NONE',  ( 0.000000000000000000, 0.000000000000000000, 1.000000000000000000 ) ) ;
#432 = VERTEX_POINT ( 'NONE', #5315 ) ;
#433 = LINE ( 'NONE', #1768, #16474 ) ;
#434 = SHAPE_REPRESENTATION ( 'circlip for shafts normal_din_Circlip DIN 471 - 10 x 1', ( #8017 ), #1061 ) ;
#435 = VERTEX_POINT ( 'NONE', #5522 ) ;
#436 = DIRECTION ( 'NONE',  ( 0.000000000000000000, 0.000000000000000000, 1.000000000000000000 ) ) ;
#437 = ORIENTED_EDGE ( 'NONE', *, *, #12143, .T. ) ;
#438 = STYLED_ITEM ( 'NONE', ( #4638 ), #574 ) ;
#439 = DIRECTION ( 'NONE',  ( 0.000000000000000000, 0.000000000000000000, 1.000000000000000000 ) ) ;
#440 = CARTESIAN_POINT ( 'NONE',  ( 0.1404048886732821022, 4.699864953788070565, -3.686887068327037387 ) ) ;
#441 = ORIENTED_EDGE ( 'NONE', *, *, #15622, .T. ) ;
#442 = ORIENTED_EDGE ( 'NONE', *, *, #7354, .T. ) ;
#443 = DIRECTION ( 'NONE',  ( -0.000000000000000000, 1.000000000000000000, -0.000000000000000000 ) ) ;
#444 = FILL_AREA_STYLE ('',( #9397 ) ) ;
#445 = VERTEX_POINT ( 'NONE', #2658 ) ;
#446 = CARTESIAN_POINT ( 'NONE',  ( -10.00000000000000000, 0.000000000000000000, 0.000000000000000000 ) ) ;
#447 = EDGE_CURVE ( 'NONE', #5630, #6042, #11910, .T. ) ;
#448 = AXIS2_PLACEMENT_3D ( 'NONE', #12033, #7849, #18129 ) ;
#449 = LINE ( 'NONE', #1790, #13535 ) ;
#450 = VECTOR ( 'NONE', #13418, 1000.000000000000000 ) ;
#451 = VERTEX_POINT ( 'NONE', #957 ) ;
#452 = EDGE_LOOP ( 'NONE', ( #14640, #10438, #12655, #9702 ) ) ;
#453 = DIRECTION ( 'NONE',  ( 1.000000000000000000, 0.000000000000000000, 0.000000000000000000 ) ) ;
#454 = CYLINDRICAL_SURFACE ( 'NONE', #8359, 24.00000000002399503 ) ;
#455 = DIRECTION ( 'NONE',  ( 0.000000000000000000, 0.000000000000000000, 1.000000000000000000 ) ) ;
#456 = EDGE_CURVE ( 'NONE', #1332, #4270, #14353, .T. ) ;
#457 = ORIENTED_EDGE ( 'NONE', *, *, #6226, .F. ) ;
#458 = DIRECTION ( 'NONE',  ( 0.000000000000000000, 1.000000000000000000, 0.000000000000000000 ) ) ;
#459 = DIRECTION ( 'NONE',  ( 0.000000000000000000, -1.000000000000000000, 0.000000000000000000 ) ) ;
#460 = CARTESIAN_POINT ( 'NONE',  ( 10.04305231718579705, -30.00000000000000000, 33.55933677959249195 ) ) ;
#461 = DIRECTION ( 'NONE',  ( 0.000000000000000000, 0.000000000000000000, 1.000000000000000000 ) ) ;
#462 = ORIENTED_EDGE ( 'NONE', *, *, #18236, .F. ) ;
#463 = CARTESIAN_POINT ( 'NONE',  ( 0.000000000000000000, -30.00000000000000000, 0.000000000000000000 ) ) ;
#464 = CYLINDRICAL_SURFACE ( 'NONE', #11147, 12.00000000001200817 ) ;
#465 = EDGE_CURVE ( 'NONE', #13362, #5083, #18469, .T. ) ;
#466 = AXIS2_PLACEMENT_3D ( 'NONE', #15273, #11070, #12708 ) ;
#467 = CIRCLE ( 'NONE', #2900, 63.00000000006298961 ) ;
#468 = ORIENTED_EDGE ( 'NONE', *, *, #14255, .T. ) ;
#469 = DIRECTION ( 'NONE',  ( -0.000000000000000000, 1.000000000000000000, -0.000000000000000000 ) ) ;
#470 = DIRECTION ( 'NONE',  ( 0.000000000000000000, 0.000000000000000000, 1.000000000000000000 ) ) ;
#471 = CIRCLE ( 'NONE', #1989, 63.00000000006298961 ) ;
#472 = B_SPLINE_CURVE_WITH_KNOTS ( 'NONE', 3,
 ( #4129, #15648, #2699, #8507, #14321, #1186, #18795, #1365 ),
 .UNSPECIFIED., .F., .F.,
 ( 4, 2, 2, 4 ),
 ( 0.005725059856848641743, 0.006314084072593626612, 0.006903108288338611481, 0.008081156719828581220 ),
 .UNSPECIFIED. ) ;
#473 = CIRCLE ( 'NONE', #160, 4.000000000000000000 ) ;
#474 = AXIS2_PLACEMENT_3D ( 'NONE', #3777, #18252, #9676 ) ;
#475 = VERTEX_POINT ( 'NONE', #13899 ) ;
#476 = EDGE_CURVE ( 'NONE', #7314, #5247, #9708, .T. ) ;
#477 = DIRECTION ( 'NONE',  ( 0.000000000000000000, 0.000000000000000000, 1.000000000000000000 ) ) ;
#478 = VERTEX_POINT ( 'NONE', #18182 ) ;
#479 = TOROIDAL_SURFACE ( 'NONE', #9907, 4.000000000000000000, 0.2500000000000000000 ) ;
#480 = DIRECTION ( 'NONE',  ( 0.000000000000000000, 0.000000000000000000, 1.000000000000000000 ) ) ;
#481 = CARTESIAN_POINT ( 'NONE',  ( -79.64793068852898728, -30.00000000000000000, -31.86039329588756530 ) ) ;
#482 = DIRECTION ( 'NONE',  ( 0.000000000000000000, 0.000000000000000000, 1.000000000000000000 ) ) ;
#483 = CARTESIAN_POINT ( 'NONE',  ( 0.000000000000000000, -58.55669782892479702, 23.24033432160416268 ) ) ;
#484 = VERTEX_POINT ( 'NONE', #14087 ) ;
#485 = CARTESIAN_POINT ( 'NONE',  ( -90.40159941089927997, 2.081668171172168513E-14, -4.983845695167307355 ) ) ;
#486 =( LENGTH_UNIT ( ) NAMED_UNIT ( * ) SI_UNIT ( .MILLI., .METRE. ) );
#487 = CARTESIAN_POINT ( 'NONE',  ( 10.00000000000000000, 55.83748330407397020, 7.813799127874245798 ) ) ;
#488 = ORIENTED_EDGE ( 'NONE', *, *, #10454, .T. ) ;
#489 = CIRCLE ( 'NONE', #2924, 2.649999999999999467 ) ;
#490 = AXIS2_PLACEMENT_3D ( 'NONE', #8974, #8892, #9173 ) ;
#491 = AXIS2_PLACEMENT_3D ( 'NONE', #7155, #9741, #8314 ) ;
#492 = ORIENTED_EDGE ( 'NONE', *, *, #2597, .T. ) ;
#493 = AXIS2_PLACEMENT_3D ( 'NONE', #10909, #12621, #9669 ) ;
#494 = AXIS2_PLACEMENT_3D ( 'NONE', #9814, #2390, #9620 ) ;
#495 = ORIENTED_EDGE ( 'NONE', *, *, #4462, .F. ) ;
#496 = EDGE_CURVE ( 'NONE', #11686, #6003, #9891, .T. ) ;
#497 = EDGE_CURVE ( 'NONE', #9138, #1316, #3398, .T. ) ;
#498 = ORIENTED_EDGE ( 'NONE', *, *, #10985, .T. ) ;
#499 = CYLINDRICAL_SURFACE ( 'NONE', #6283, 63.00000000006298961 ) ;
#500 = ADVANCED_FACE ( 'NONE', ( #12472 ), #2370, .T. ) ;
#501 = SURFACE_SIDE_STYLE ('',( #12015 ) ) ;
#502 = AXIS2_PLACEMENT_3D ( 'NONE', #14003, #960, #12568 ) ;
#503 = CIRCLE ( 'NONE', #18134, 63.00000000006298961 ) ;
#504 = DIRECTION ( 'NONE',  ( 0.000000000000000000, 0.7071067811865436870, 0.7071067811865513475 ) ) ;
#505 = DIRECTION ( 'NONE',  ( -0.000000000000000000, 1.000000000000000000, -0.000000000000000000 ) ) ;
#506 = CIRCLE ( 'NONE', #15414, 5.000000000000004441 ) ;
#507 = EDGE_CURVE ( 'NONE', #3158, #1316, #8188, .T. ) ;
#508 = LINE ( 'NONE', #698, #14239 ) ;
#509 = CARTESIAN_POINT ( 'NONE',  ( 10.00000000000000000, 0.000000000000000000, 0.000000000000000000 ) ) ;
#510 = AXIS2_PLACEMENT_3D ( 'NONE', #13465, #13552, #17930 ) ;
#511 = CARTESIAN_POINT ( 'NONE',  ( 11.14999999999999680, 0.000000000000000000, 0.000000000000000000 ) ) ;
#512 = ORIENTED_EDGE ( 'NONE', *, *, #112, .F. ) ;
#513 = DIRECTION ( 'NONE',  ( 0.000000000000000000, 0.000000000000000000, 1.000000000000000000 ) ) ;
#514 = VERTEX_POINT ( 'NONE', #12562 ) ;
#515 = ADVANCED_FACE ( 'NONE', ( #11123 ), #8371, .T. ) ;
#516 = CARTESIAN_POINT ( 'NONE',  ( 10.00000000000000000, 0.000000000000000000, -1.500000000000000000 ) ) ;
#517 = CARTESIAN_POINT ( 'NONE',  ( 10.00000000000000000, -27.72801475327285559, 5.086963483077107995 ) ) ;
#518 = EDGE_CURVE ( 'NONE', #10933, #833, #10392, .T. ) ;
#519 = CARTESIAN_POINT ( 'NONE',  ( 50.00005079999999680, 6.799999999999999822, -1.500000000000000000 ) ) ;
#520 = ORIENTED_EDGE ( 'NONE', *, *, #14011, .T. ) ;
#521 = ORIENTED_EDGE ( 'NONE', *, *, #9953, .T. ) ;
#522 = DIRECTION ( 'NONE',  ( 0.000000000000000000, 0.000000000000000000, 1.000000000000000000 ) ) ;
#523 = CARTESIAN_POINT ( 'NONE',  ( 13.90576474687299680, 15.00000000000001599, 42.79754323328179311 ) ) ;
#524 = EDGE_CURVE ( 'NONE', #2625, #7275, #2184, .T. ) ;
#525 = CARTESIAN_POINT ( 'NONE',  ( -2.805705207896067144, 3.226868319750155312, -3.503898532754364581 ) ) ;
#526 = ORIENTED_EDGE ( 'NONE', *, *, #16492, .F. ) ;
#527 = CIRCLE ( 'NONE', #8139, 28.00000000000000355 ) ;
#528 = AXIS2_PLACEMENT_3D ( 'NONE', #15509, #8361, #6654 ) ;
#529 = AXIS2_PLACEMENT_3D ( 'NONE', #16197, #4487, #18349 ) ;
#530 = AXIS2_PLACEMENT_3D ( 'NONE', #4970, #11933, #16504 ) ;
#531 = EDGE_CURVE ( 'NONE', #4599, #15674, #9181, .T. ) ;
#532 = CARTESIAN_POINT ( 'NONE',  ( -3.309651814758565180, -5.455921364805393026, 0.000000000000000000 ) ) ;
#533 = CARTESIAN_POINT ( 'NONE',  ( 129.9999999999999432, -34.99999999999999289, -125.0000000000000000 ) ) ;
#534 = DIRECTION ( 'NONE',  ( 1.000000000000000000, -0.000000000000000000, -0.000000000000000000 ) ) ;
#535 = ORIENTED_EDGE ( 'NONE', *, *, #4870, .T. ) ;
#536 = FACE_BOUND ( 'NONE', #6514, .T. ) ;
#537 = VECTOR ( 'NONE', #11015, 1000.000000000000000 ) ;
#538 = VERTEX_POINT ( 'NONE', #10338 ) ;
#539 = DIRECTION ( 'NONE',  ( 1.000000000000000000, 0.000000000000000000, 0.000000000000000000 ) ) ;
#540 = EDGE_LOOP ( 'NONE', ( #9099, #3031, #14375, #5789 ) ) ;
#541 = EDGE_CURVE ( 'NONE', #11202, #728, #9483, .T. ) ;
#542 = VECTOR ( 'NONE', #17182, 1000.000000000000000 ) ;
#543 = DIRECTION ( 'NONE',  ( 0.000000000000000000, 0.000000000000000000, -1.000000000000000000 ) ) ;
#544 = CARTESIAN_POINT ( 'NONE',  ( -2.807080416178626692, 3.225969019225154444, -3.502507215260441065 ) ) ;
#545 = AXIS2_PLACEMENT_3D ( 'NONE', #3110, #11499, #10065 ) ;
#546 = ORIENTED_EDGE ( 'NONE', *, *, #4687, .T. ) ;
#547 = ORIENTED_EDGE ( 'NONE', *, *, #996, .F. ) ;
#548 = AXIS2_PLACEMENT_3D ( 'NONE', #1931, #7836, #7731 ) ;
#549 = LINE ( 'NONE', #1872, #13865 ) ;
#550 = ORIENTED_EDGE ( 'NONE', *, *, #5972, .T. ) ;
#551 = CARTESIAN_POINT ( 'NONE',  ( 0.3865131578947368918, -23.49682122285426189, -2.000000000000000000 ) ) ;
#552 = CARTESIAN_POINT ( 'NONE',  ( 4.236525694536557474, -2.416953475386482530, -3.751298745799839462 ) ) ;
#553 = AXIS2_PLACEMENT_3D ( 'NONE', #134, #7279, #17465 ) ;
#554 = ORIENTED_EDGE ( 'NONE', *, *, #177, .T. ) ;
#555 = PRODUCT_DEFINITION_SHAPE ( 'NONE', 'NONE',  #18838 ) ;
#556 = ORIENTED_EDGE ( 'NONE', *, *, #3480, .T. ) ;
#557 = CARTESIAN_POINT ( 'NONE',  ( 0.000000000000000000, -26.71881558261694778, -49.49802920186251498 ) ) ;
#558 = CARTESIAN_POINT ( 'NONE',  ( 0.000000000000000000, -13.79392154159090111, -61.47135697633794393 ) ) ;
#559 = LINE ( 'NONE', #10649, #2964 ) ;
#560 = VERTEX_POINT ( 'NONE', #17852 ) ;
#561 = FACE_OUTER_BOUND ( 'NONE', #18564, .T. ) ;
#562 = EDGE_CURVE ( 'NONE', #1723, #7149, #1596, .T. ) ;
#563 = CARTESIAN_POINT ( 'NONE',  ( -90.00000000009001155, -10.00000000000001599, -1.301042606982603940E-15 ) ) ;
#564 = CYLINDRICAL_SURFACE ( 'NONE', #2820, 7.500000000000007105 ) ;
#565 = VECTOR ( 'NONE', #11959, 1000.000000000000000 ) ;
#566 = CARTESIAN_POINT ( 'NONE',  ( 10.00000000000000000, 27.72801475327282361, 6.913036516934699449 ) ) ;
#567 = EDGE_LOOP ( 'NONE', ( #6055, #18455, #17783, #6474 ) ) ;
#568 = CYLINDRICAL_SURFACE ( 'NONE', #2631, 63.00000000006298961 ) ;
#569 = ORIENTED_EDGE ( 'NONE', *, *, #13463, .T. ) ;
#570 = DIRECTION ( 'NONE',  ( 1.000000000000000000, 0.000000000000000000, 0.000000000000000000 ) ) ;
#571 = CARTESIAN_POINT ( 'NONE',  ( 10.00000000000000000, 61.03368945066435458, 15.61693798565518421 ) ) ;
#572 = CIRCLE ( 'NONE', #17307, 1.250000000000001110 ) ;
#573 = CIRCLE ( 'NONE', #10906, 33.00000000003299760 ) ;
#574 = ADVANCED_BREP_SHAPE_REPRESENTATION ( '', ( #3243, #8017 ), #16563 ) ;
#575 = AXIS2_PLACEMENT_3D ( 'NONE', #233, #3180, #513 ) ;
#576 = EDGE_LOOP ( 'NONE', ( #11256, #8349, #6691, #4842 ) ) ;
#577 = CIRCLE ( 'NONE', #3336, 5.560781378645573980 ) ;
#578 = EDGE_CURVE ( 'NONE', #13109, #8902, #3719, .T. ) ;
#579 = AXIS2_PLACEMENT_3D ( 'NONE', #4765, #8860, #4862 ) ;
#580 = EDGE_LOOP ( 'NONE', ( #11778, #1324 ) ) ;
#581 = CIRCLE ( 'NONE', #11233, 2.500000000000000888 ) ;
#582 = CARTESIAN_POINT ( 'NONE',  ( 4.211399257449709665, -2.459727064652517114, -3.751161691472417736 ) ) ;
#583 = DIRECTION ( 'NONE',  ( 0.000000000000000000, 0.000000000000000000, 1.000000000000000000 ) ) ;
#584 = CARTESIAN_POINT ( 'NONE',  ( -31.74999999999995737, 5.204748896376250699E-16, -4.250000000000000000 ) ) ;
#585 = CYLINDRICAL_SURFACE ( 'NONE', #13933, 33.00000000003299760 ) ;
#586 = DIRECTION ( 'NONE',  ( -1.000000000000000000, 0.000000000000000000, -0.000000000000000000 ) ) ;
#587 = ORIENTED_EDGE ( 'NONE', *, *, #5226, .T. ) ;
#588 = CYLINDRICAL_SURFACE ( 'NONE', #9094, 56.24900000005625600 ) ;
#589 = DIRECTION ( 'NONE',  ( 1.000000000000000000, 0.000000000000000000, 0.000000000000000000 ) ) ;
#590 = AXIS2_PLACEMENT_3D ( 'NONE', #16022, #7347, #5916 ) ;
#591 = ORIENTED_EDGE ( 'NONE', *, *, #16105, .F. ) ;
#592 = ITEM_DEFINED_TRANSFORMATION ( 'NONE', 'NONE', #5624,  #8017 ) ;
#593 = CIRCLE ( 'NONE', #16724, 63.00000000006298961 ) ;
#594 = ORIENTED_EDGE ( 'NONE', *, *, #13827, .T. ) ;
#595 = ORIENTED_EDGE ( 'NONE', *, *, #18213, .F. ) ;
#596 = VERTEX_POINT ( 'NONE', #6138 ) ;
#597 = CARTESIAN_POINT ( 'NONE',  ( -90.38553543446691663, 1.000000000000018208, -4.784491867360616268 ) ) ;
#598 = CARTESIAN_POINT ( 'NONE',  ( -79.64793068852927149, -38.00000000000000000, 34.51039329588763849 ) ) ;
#599 = CIRCLE ( 'NONE', #2110, 33.00000000003299760 ) ;
#600 = CARTESIAN_POINT ( 'NONE',  ( -56.50000000009000445, -34.99999999999999289, 3.817814120399276590E-13 ) ) ;
#601 = CARTESIAN_POINT ( 'NONE',  ( -90.00000000009001155, -13.00000000000001776, -1.691355389077386325E-15 ) ) ;
#602 = AXIS2_PLACEMENT_3D ( 'NONE', #15281, #16437, #16812 ) ;
#603 = CARTESIAN_POINT ( 'NONE',  ( 5.000000000000004441, 5.204748896376250699E-16, -4.250000000000000000 ) ) ;
#604 = DIRECTION ( 'NONE',  ( 0.000000000000000000, 0.000000000000000000, 1.000000000000000000 ) ) ;
#605 = DIRECTION ( 'NONE',  ( 0.000000000000000000, 0.000000000000000000, -1.000000000000000000 ) ) ;
#606 = CYLINDRICAL_SURFACE ( 'NONE', #1990, 56.24900000005625600 ) ;
#607 = VERTEX_POINT ( 'NONE', #6230 ) ;
#608 = FACE_OUTER_BOUND ( 'NONE', #1873, .T. ) ;
#609 = ORIENTED_EDGE ( 'NONE', *, *, #12136, .F. ) ;
#610 = DIRECTION ( 'NONE',  ( 0.000000000000000000, 0.000000000000000000, 1.000000000000000000 ) ) ;
#611 = CARTESIAN_POINT ( 'NONE',  ( -4.197393957002303999, -7.773935952363655451E-14, -3.503767560748929810 ) ) ;
#612 = DIRECTION ( 'NONE',  ( -0.7071067811865364705, 8.659560562355067211E-17, -0.7071067811865584529 ) ) ;
#613 = ORIENTED_EDGE ( 'NONE', *, *, #5750, .F. ) ;
#614 = EDGE_LOOP ( 'NONE', ( #7993, #13909, #15314, #4933 ) ) ;
#615 = EDGE_CURVE ( 'NONE', #3160, #417, #7117, .T. ) ;
#616 = CYLINDRICAL_SURFACE ( 'NONE', #6258, 2.649999999999999467 ) ;
#617 = DIRECTION ( 'NONE',  ( 0.000000000000000000, 0.000000000000000000, 1.000000000000000000 ) ) ;
#619 = EDGE_CURVE ( 'NONE', #16309, #3893, #687, .T. ) ;
#618 = CARTESIAN_POINT ( 'NONE',  ( 10.00000000000000000, -13.79392154159089756, -61.47135697633793683 ) ) ;
#620 = EDGE_LOOP ( 'NONE', ( #239, #4608, #6454, #6087 ) ) ;
#621 = CIRCLE ( 'NONE', #2138, 33.00000000003299760 ) ;
#622=STYLED_ITEM('',(#18869),#9854);
#623 = ADVANCED_FACE ( 'NONE', ( #3105 ), #12035, .T. ) ;
#624 = ADVANCED_FACE ( 'NONE', ( #11857 ), #1293, .F. ) ;
#625 = DIRECTION ( 'NONE',  ( 0.000000000000000000, 0.000000000000000000, 1.000000000000000000 ) ) ;
#626 = LINE ( 'NONE', #18240, #10043 ) ;
#627 = CARTESIAN_POINT ( 'NONE',  ( 10.00000000000000000, 62.87238730325621106, -4.007856633823605463 ) ) ;
#628 = ORIENTED_EDGE ( 'NONE', *, *, #3896, .T. ) ;
#629 = CARTESIAN_POINT ( 'NONE',  ( -10.00000000000000000, 0.000000000000000000, 0.000000000000000000 ) ) ;
#630 = EDGE_CURVE ( 'NONE', #2530, #13928, #2807, .T. ) ;
#631 = ORIENTED_EDGE ( 'NONE', *, *, #7642, .T. ) ;
#632 = UNCERTAINTY_MEASURE_WITH_UNIT (LENGTH_MEASURE( 1.000000000000000082E-05 ), #16986, 'distance_accuracy_value', 'NONE');
#633 = CARTESIAN_POINT ( 'NONE',  ( 10.00000000000000000, 27.72801475327282361, -5.086963483077305170 ) ) ;
#634 = ORIENTED_EDGE ( 'NONE', *, *, #3408, .F. ) ;
#635 =( REPRESENTATION_RELATIONSHIP ('NONE','NONE', #11014, #2517 ) REPRESENTATION_RELATIONSHIP_WITH_TRANSFORMATION ( #8109 )SHAPE_REPRESENTATION_RELATIONSHIP( ) );
#636 = VECTOR ( 'NONE', #11597, 1000.000000000000000 ) ;
#637 = DIRECTION ( 'NONE',  ( -1.000000000000000000, 0.000000000000000000, 0.000000000000000000 ) ) ;
#638 = CARTESIAN_POINT ( 'NONE',  ( 10.00000000000000000, -42.79754323328189969, -13.90576474687263264 ) ) ;
#639 = ORIENTED_EDGE ( 'NONE', *, *, #13733, .F. ) ;
#640 = ORIENTED_EDGE ( 'NONE', *, *, #15047, .T. ) ;
#641 = EDGE_CURVE ( 'NONE', #14362, #16890, #13288, .T. ) ;
#642 = CARTESIAN_POINT ( 'NONE',  ( 10.00000000000000000, 0.000000000000000000, 0.000000000000000000 ) ) ;
#643 =( NAMED_UNIT ( * ) PLANE_ANGLE_UNIT ( ) SI_UNIT ( $, .RADIAN. ) );
#644 = EDGE_CURVE ( 'NONE', #280, #4113, #4330, .T. ) ;
#645 = VERTEX_POINT ( 'NONE', #15002 ) ;
#646 = LINE ( 'NONE', #15390, #12767 ) ;
#647 = ADVANCED_FACE ( 'NONE', ( #12940 ), #11765, .T. ) ;
#648 = EDGE_CURVE ( 'NONE', #13033, #17129, #9085, .T. ) ;
#649 = AXIS2_PLACEMENT_3D ( 'NONE', #4437, #7479, #13300 ) ;
#650 = DIRECTION ( 'NONE',  ( -1.000000000000000000, -0.000000000000000000, -0.000000000000000000 ) ) ;
#651 = CARTESIAN_POINT ( 'NONE',  ( 10.00000000000000000, -27.94286728106395756, 15.73043801031622912 ) ) ;
#652 = VERTEX_POINT ( 'NONE', #4706 ) ;
#653 = ORIENTED_EDGE ( 'NONE', *, *, #10856, .F. ) ;
#654 = DIRECTION ( 'NONE',  ( 0.000000000000000000, 0.000000000000000000, -1.000000000000000000 ) ) ;
#655 = CARTESIAN_POINT ( 'NONE',  ( 0.000000000000000000, -61.03368945066446827, 15.61693798565473656 ) ) ;
#656 = CARTESIAN_POINT ( 'NONE',  ( -0.3865131578947368918, -23.49682122285426189, 0.000000000000000000 ) ) ;
#657 = VERTEX_POINT ( 'NONE', #4189 ) ;
#658 = CARTESIAN_POINT ( 'NONE',  ( 0.000000000000000000, 1.335003989222417697, -56.23315539212688918 ) ) ;
#659 = DIRECTION ( 'NONE',  ( -1.000000000000000000, -0.000000000000000000, -0.000000000000000000 ) ) ;
#660 = DIRECTION ( 'NONE',  ( -1.000000000000000000, 0.000000000000000000, -0.000000000000000000 ) ) ;
#661 = DIRECTION ( 'NONE',  ( 1.000000000000000000, -0.000000000000000000, 0.000000000000000000 ) ) ;
#662 = ORIENTED_EDGE ( 'NONE', *, *, #2383, .T. ) ;
#663 = AXIS2_PLACEMENT_3D ( 'NONE', #15792, #17214, #4171 ) ;
#664 = CARTESIAN_POINT ( 'NONE',  ( 10.00000000000000000, -31.97297851452457351, 46.27827401617392411 ) ) ;
#665 = EDGE_LOOP ( 'NONE', ( #4697, #15423, #2436, #2254 ) ) ;
#666 = CARTESIAN_POINT ( 'NONE',  ( 5.200000000000002842, 0.000000000000000000, 0.000000000000000000 ) ) ;
#667 = CARTESIAN_POINT ( 'NONE',  ( 5.000000000000000000, 4.381479206522992165, 32.70783759231088084 ) ) ;
#668 = CIRCLE ( 'NONE', #12855, 24.00000000002400569 ) ;
#669 = EDGE_CURVE ( 'NONE', #2958, #2652, #11537, .T. ) ;
#670 = ORIENTED_EDGE ( 'NONE', *, *, #3951, .F. ) ;
#671 = ORIENTED_EDGE ( 'NONE', *, *, #1460, .F. ) ;
#672 = FACE_OUTER_BOUND ( 'NONE', #6327, .T. ) ;
#673 = CARTESIAN_POINT ( 'NONE',  ( 3.999999999999998224, 2.472263674411418588, -3.687027874309861897 ) ) ;
#674 = FACE_OUTER_BOUND ( 'NONE', #9063, .T. ) ;
#675 = DIRECTION ( 'NONE',  ( 1.000000000000000000, -0.000000000000000000, 0.000000000000000000 ) ) ;
#676 = AXIS2_PLACEMENT_3D ( 'NONE', #14556, #1514, #13044 ) ;
#677 = DIRECTION ( 'NONE',  ( 1.000000000000000000, 0.000000000000000000, 0.000000000000000000 ) ) ;
#678 = CARTESIAN_POINT ( 'NONE',  ( 0.000000000000000000, 0.000000000000000000, -4.974599999999998801 ) ) ;
#679 = ORIENTED_EDGE ( 'NONE', *, *, #1431, .F. ) ;
#680 = DIRECTION ( 'NONE',  ( 0.000000000000000000, 0.000000000000000000, -1.000000000000000000 ) ) ;
#681 = EDGE_CURVE ( 'NONE', #6992, #16250, #13353, .T. ) ;
#682 = PRESENTATION_STYLE_ASSIGNMENT (( #9797 ) ) ;
#683 = CARTESIAN_POINT ( 'NONE',  ( 0.000000000000000000, 0.000000000000000000, 0.000000000000000000 ) ) ;
#684 = VERTEX_POINT ( 'NONE', #16240 ) ;
#685 = CONTEXT_DEPENDENT_SHAPE_REPRESENTATION ( #16560, #18041 ) ;
#686 = EDGE_CURVE ( 'NONE', #12093, #4981, #3289, .T. ) ;
#687 = CIRCLE ( 'NONE', #9492, 63.00000000006298961 ) ;
#688 = ORIENTED_EDGE ( 'NONE', *, *, #12289, .T. ) ;
#689 = AXIS2_PLACEMENT_3D ( 'NONE', #18645, #7031, #2265 ) ;
#690 = ORIENTED_EDGE ( 'NONE', *, *, #12876, .F. ) ;
#691 = AXIS2_PLACEMENT_3D ( 'NONE', #509, #9078, #10601 ) ;
#692 = ORIENTED_EDGE ( 'NONE', *, *, #5967, .F. ) ;
#693 = DIRECTION ( 'NONE',  ( 1.000000000000000000, 0.000000000000000000, 0.000000000000000000 ) ) ;
#694 = CARTESIAN_POINT ( 'NONE',  ( 0.000000000000000000, -1.178949249685218081, -2.041999999999998039 ) ) ;
#695 = DIRECTION ( 'NONE',  ( 0.000000000000000000, 0.000000000000000000, 1.000000000000000000 ) ) ;
#696 = LINE ( 'NONE', #18305, #3229 ) ;
#697 = CARTESIAN_POINT ( 'NONE',  ( -10.00000000000000000, 0.000000000000000000, 0.000000000000000000 ) ) ;
#698 = CARTESIAN_POINT ( 'NONE',  ( -4.249769933734879324, -30.10148593525447680, -2.000000000000000000 ) ) ;
#699 = DIRECTION ( 'NONE',  ( 1.000000000000000000, 0.000000000000000000, 0.000000000000000000 ) ) ;
#700 = FACE_OUTER_BOUND ( 'NONE', #13011, .T. ) ;
#701 = VERTEX_POINT ( 'NONE', #3192 ) ;
#702 = CYLINDRICAL_SURFACE ( 'NONE', #5436, 26.24900000002624978 ) ;
#703 = ORIENTED_EDGE ( 'NONE', *, *, #8448, .F. ) ;
#704 = EDGE_CURVE ( 'NONE', #7573, #2619, #14807, .T. ) ;
#705 = EDGE_CURVE ( 'NONE', #15024, #931, #15786, .T. ) ;
#706 = CIRCLE ( 'NONE', #11348, 2.649999999999992806 ) ;
#707 = CARTESIAN_POINT ( 'NONE',  ( 10.00000000000000000, -26.49895292618039377, 49.76630880786299826 ) ) ;
#708 = FACE_BOUND ( 'NONE', #15504, .T. ) ;
#709 = ORIENTED_EDGE ( 'NONE', *, *, #3804, .F. ) ;
#710 = ORIENTED_EDGE ( 'NONE', *, *, #5586, .F. ) ;
#711 = AXIS2_PLACEMENT_3D ( 'NONE', #11816, #4571, #11718 ) ;
#712 = DIRECTION ( 'NONE',  ( 0.000000000000000000, 0.000000000000000000, 1.000000000000000000 ) ) ;
#713 = DIRECTION ( 'NONE',  ( 0.9938152567191714803, 0.000000000000000000, -0.1110460963393456596 ) ) ;
#714 = EDGE_CURVE ( 'NONE', #10711, #18131, #266, .T. ) ;
#715 = DIRECTION ( 'NONE',  ( 0.000000000000000000, 0.000000000000000000, 1.000000000000000000 ) ) ;
#716 = ORIENTED_EDGE ( 'NONE', *, *, #12750, .F. ) ;
#717 = EDGE_CURVE ( 'NONE', #18313, #13820, #6667, .T. ) ;
#718 = CIRCLE ( 'NONE', #11362, 2.649999999999995914 ) ;
#719 = CARTESIAN_POINT ( 'NONE',  ( 5.000000000000000000, -61.47135697633769524, -13.79392154159199713 ) ) ;
#720 = CARTESIAN_POINT ( 'NONE',  ( 0.000000000000000000, -34.99999999999999289, 0.000000000000000000 ) ) ;
#721 = DIRECTION ( 'NONE',  ( 1.000000000000000000, 0.000000000000000000, 0.000000000000000000 ) ) ;
#722 = ORIENTED_EDGE ( 'NONE', *, *, #18740, .F. ) ;
#723 = ADVANCED_FACE ( 'NONE', ( #3576 ), #9271, .T. ) ;
#724 = DIRECTION ( 'NONE',  ( -1.000000000000000000, 0.000000000000000000, 0.000000000000000000 ) ) ;
#725 = EDGE_CURVE ( 'NONE', #9332, #10957, #11102, .T. ) ;
#726 = VERTEX_POINT ( 'NONE', #2047 ) ;
#727 = DIRECTION ( 'NONE',  ( 0.000000000000000000, 0.000000000000000000, 1.000000000000000000 ) ) ;
#728 = VERTEX_POINT ( 'NONE', #12518 ) ;
#729 = EDGE_CURVE ( 'NONE', #10240, #1960, #467, .T. ) ;
#730 = ADVANCED_FACE ( 'NONE', ( #12316 ), #15275, .T. ) ;
#731 = CYLINDRICAL_SURFACE ( 'NONE', #17532, 33.00000000003299760 ) ;
#732 = DIRECTION ( 'NONE',  ( -1.000000000000000000, 0.000000000000000000, 0.000000000000000000 ) ) ;
#733 = ORIENTED_EDGE ( 'NONE', *, *, #13326, .T. ) ;
#734 = EDGE_LOOP ( 'NONE', ( #4079, #5320, #4537, #1238 ) ) ;
#735 = DIRECTION ( 'NONE',  ( 0.000000000000000000, -0.5877852522924801315, 0.8090169943749422332 ) ) ;
#736 =( NAMED_UNIT ( * ) SI_UNIT ( $, .STERADIAN. ) SOLID_ANGLE_UNIT ( ) );
#737 =( GEOMETRIC_REPRESENTATION_CONTEXT ( 3 ) GLOBAL_UNCERTAINTY_ASSIGNED_CONTEXT ( ( #6522 ) ) GLOBAL_UNIT_ASSIGNED_CONTEXT ( ( #17644, #7438, #13541 ) ) REPRESENTATION_CONTEXT ( 'NONE', 'WORKASPACE' ) );
#738 = ORIENTED_EDGE ( 'NONE', *, *, #1656, .F. ) ;
#739 = CARTESIAN_POINT ( 'NONE',  ( -10.00000000000000000, 0.000000000000000000, 0.000000000000000000 ) ) ;
#740 = EDGE_CURVE ( 'NONE', #12029, #728, #5327, .T. ) ;
#741 = FACE_OUTER_BOUND ( 'NONE', #7620, .T. ) ;
#742 = DIRECTION ( 'NONE',  ( -0.000000000000000000, -0.000000000000000000, -1.000000000000000000 ) ) ;
#743 = VERTEX_POINT ( 'NONE', #618 ) ;
#744 = EDGE_CURVE ( 'NONE', #4042, #7876, #15574, .T. ) ;
#745 = STYLED_ITEM ( 'NONE', ( #16686 ), #12609 ) ;
#746 = EDGE_CURVE ( 'NONE', #9477, #9087, #6433, .T. ) ;
#747 = EDGE_CURVE ( 'NONE', #16326, #1501, #17400, .T. ) ;
#748 = ORIENTED_EDGE ( 'NONE', *, *, #17754, .T. ) ;
#749 = CARTESIAN_POINT ( 'NONE',  ( -11.25000000000000355, 0.000000000000000000, -27.00000000000000355 ) ) ;
#750 = CARTESIAN_POINT ( 'NONE',  ( 0.000000000000000000, -62.87238730325623948, 4.007856633823172032 ) ) ;
#751 = CARTESIAN_POINT ( 'NONE',  ( 0.000000000000000000, 0.000000000000000000, 0.000000000000000000 ) ) ;
#752 = VERTEX_POINT ( 'NONE', #4902 ) ;
#753 = CARTESIAN_POINT ( 'NONE',  ( 2.500000000000000000, -1.178949249685213863, 2.042000000000001148 ) ) ;
#754 = EDGE_CURVE ( 'NONE', #8328, #17358, #3852, .T. ) ;
#755 = DIRECTION ( 'NONE',  ( 0.000000000000000000, 0.8910065241883688980, -0.4539904997395446951 ) ) ;
#756 = DIRECTION ( 'NONE',  ( 0.000000000000000000, 0.000000000000000000, 1.000000000000000000 ) ) ;
#757 = ORIENTED_EDGE ( 'NONE', *, *, #10060, .F. ) ;
#758 = DIRECTION ( 'NONE',  ( -1.000000000000000000, 0.000000000000000000, 0.000000000000000000 ) ) ;
#759 = ORIENTED_EDGE ( 'NONE', *, *, #6952, .F. ) ;
#760 = CARTESIAN_POINT ( 'NONE',  ( -94.77031323234206184, 1.000000000000018208, 0.5330212624288541701 ) ) ;
#761 = ORIENTED_EDGE ( 'NONE', *, *, #2237, .T. ) ;
#762 = DIRECTION ( 'NONE',  ( -1.000000000000000000, -0.000000000000000000, -0.000000000000000000 ) ) ;
#763 = DIRECTION ( 'NONE',  ( 0.000000000000000000, 0.000000000000000000, -1.000000000000000000 ) ) ;
#764 = EDGE_CURVE ( 'NONE', #3720, #10887, #3348, .T. ) ;
#765 = AXIS2_PLACEMENT_3D ( 'NONE', #14091, #5531, #7226 ) ;
#766 = ORIENTED_EDGE ( 'NONE', *, *, #14475, .F. ) ;
#767 = EDGE_CURVE ( 'NONE', #3669, #4773, #5758, .T. ) ;
#768 = ORIENTED_EDGE ( 'NONE', *, *, #17161, .T. ) ;
#769 = DIRECTION ( 'NONE',  ( 0.000000000000000000, 0.000000000000000000, 1.000000000000000000 ) ) ;
#770 = DIRECTION ( 'NONE',  ( -1.000000000000000000, 0.000000000000000000, 0.000000000000000000 ) ) ;
#771 = CARTESIAN_POINT ( 'NONE',  ( 10.00000000000000178, 4.769696007084728073, -1.500000000000000000 ) ) ;
#772 = DIRECTION ( 'NONE',  ( -1.000000000000000000, 0.000000000000000000, 0.000000000000000000 ) ) ;
#773 = PRODUCT_DEFINITION_FORMATION_WITH_SPECIFIED_SOURCE ( 'ANY', '', #8595, .NOT_KNOWN. ) ;
#774 = DIRECTION ( 'NONE',  ( -1.000000000000000000, 0.000000000000000000, 0.000000000000000000 ) ) ;
#775 = CIRCLE ( 'NONE', #16575, 33.00000000003299760 ) ;
#776 = CARTESIAN_POINT ( 'NONE',  ( -90.00000000009001155, -49.14213562373095812, -5.000000000000005329 ) ) ;
#777 = ORIENTED_EDGE ( 'NONE', *, *, #16572, .T. ) ;
#778 = CARTESIAN_POINT ( 'NONE',  ( 10.00000000000000000, 0.000000000000000000, 0.000000000000000000 ) ) ;
#779 = AXIS2_PLACEMENT_3D ( 'NONE', #6879, #12893, #15840 ) ;
#780 = EDGE_CURVE ( 'NONE', #16201, #10824, #11466, .T. ) ;
#781 = CARTESIAN_POINT ( 'NONE',  ( -4.000000000000000000, -0.3979232138631226823, -3.896351557369779711E-17 ) ) ;
#782 = ORIENTED_EDGE ( 'NONE', *, *, #1620, .F. ) ;
#783 = ORIENTED_EDGE ( 'NONE', *, *, #6803, .T. ) ;
#784 = CONICAL_SURFACE ( 'NONE', #835, 2.500000000000000888, 0.9599310885968785900 ) ;
#785 = EDGE_LOOP ( 'NONE', ( #13312, #6543 ) ) ;
#786 = AXIS2_PLACEMENT_3D ( 'NONE', #10064, #2821, #8624 ) ;
#787 = AXIS2_PLACEMENT_3D ( 'NONE', #12286, #18289, #16680 ) ;
#788 = ORIENTED_EDGE ( 'NONE', *, *, #9868, .T. ) ;
#789 = CARTESIAN_POINT ( 'NONE',  ( 10.00000000000000000, -55.33199130079777461, -10.11537145609435306 ) ) ;
#790 = CARTESIAN_POINT ( 'NONE',  ( 32.50000000000000000, -26.50000000000000000, -2.649999999999631317 ) ) ;
#791 = FACE_OUTER_BOUND ( 'NONE', #14669, .T. ) ;
#792 = DIRECTION ( 'NONE',  ( 0.000000000000000000, 0.000000000000000000, 1.000000000000000000 ) ) ;
#793 = DIRECTION ( 'NONE',  ( -1.000000000000000000, 0.000000000000000000, -0.000000000000000000 ) ) ;
#794 = CARTESIAN_POINT ( 'NONE',  ( 0.000000000000000000, -49.76630880786327538, 26.49895292617986797 ) ) ;
#795 = LINE ( 'NONE', #18309, #10102 ) ;
#796 = AXIS2_PLACEMENT_3D ( 'NONE', #12535, #16739, #5001 ) ;
#797 = CARTESIAN_POINT ( 'NONE',  ( -90.00000000009001155, -38.00000000000000000, 40.00000000000000000 ) ) ;
#798 = ORIENTED_EDGE ( 'NONE', *, *, #12607, .T. ) ;
#799 = DIRECTION ( 'NONE',  ( 1.000000000000000000, 0.000000000000000000, 0.000000000000000000 ) ) ;
#800 = AXIS2_PLACEMENT_3D ( 'NONE', #11341, #18486, #12677 ) ;
#801 = ORIENTED_EDGE ( 'NONE', *, *, #4462, .T. ) ;
#802 = B_SPLINE_CURVE_WITH_KNOTS ( 'NONE', 3,
 ( #3372, #6127, #1400, #7646, #7204 ),
 .UNSPECIFIED., .F., .F.,
 ( 4, 1, 4 ),
 ( 0.000000000000000000, 0.002309401076758505356, 0.004618802153517010713 ),
 .UNSPECIFIED. ) ;
#803 = EDGE_CURVE ( 'NONE', #11858, #8925, #7390, .T. ) ;
#804 = PLANE ( 'NONE',  #2228 ) ;
#805 = DIRECTION ( 'NONE',  ( -1.000000000000000000, 0.000000000000000000, 0.000000000000000000 ) ) ;
#806 = VERTEX_POINT ( 'NONE', #6331 ) ;
#807 = CIRCLE ( 'NONE', #9610, 6.080745460913608902 ) ;
#808 = VERTEX_POINT ( 'NONE', #14043 ) ;
#809 = CIRCLE ( 'NONE', #5971, 2.649999999999999467 ) ;
#810 = CIRCLE ( 'NONE', #12974, 24.00000000002399858 ) ;
#811 = DIRECTION ( 'NONE',  ( 0.000000000000000000, 1.000000000000000000, -1.224646799147353207E-16 ) ) ;
#812 = DIRECTION ( 'NONE',  ( -1.000000000000000000, 0.000000000000000000, 0.000000000000000000 ) ) ;
#813 = ORIENTED_EDGE ( 'NONE', *, *, #41, .F. ) ;
#814 = CIRCLE ( 'NONE', #9625, 10.00000000000000888 ) ;
#815 = EDGE_CURVE ( 'NONE', #11178, #15913, #15657, .T. ) ;
#816 = AXIS2_PLACEMENT_3D ( 'NONE', #18020, #17933, #4886 ) ;
#817 = CARTESIAN_POINT ( 'NONE',  ( 0.000000000000000000, 6.799999999999999822, 0.000000000000000000 ) ) ;
#818 = FACE_BOUND ( 'NONE', #15309, .T. ) ;
#819 = CIRCLE ( 'NONE', #9937, 25.00000000000000000 ) ;
#820 = AXIS2_PLACEMENT_3D ( 'NONE', #962, #5232, #12193 ) ;
#821 = DIRECTION ( 'NONE',  ( -1.000000000000000000, -0.000000000000000000, -0.000000000000000000 ) ) ;
#822 = ORIENTED_EDGE ( 'NONE', *, *, #2491, .F. ) ;
#823 = CARTESIAN_POINT ( 'NONE',  ( 5.000000000000000888, 4.250000000000000000, 0.000000000000000000 ) ) ;
#824 = EDGE_CURVE ( 'NONE', #3056, #8661, #8769, .T. ) ;
#825 = ORIENTED_EDGE ( 'NONE', *, *, #3033, .T. ) ;
#826 = UNCERTAINTY_MEASURE_WITH_UNIT (LENGTH_MEASURE( 1.000000000000000082E-05 ), #11317, 'distance_accuracy_value', 'NONE');
#827 = CARTESIAN_POINT ( 'NONE',  ( 10.00000000000000000, 5.876895005582430720, 62.72529079327808432 ) ) ;
#828 = ORIENTED_EDGE ( 'NONE', *, *, #3325, .T. ) ;
#829 = DIRECTION ( 'NONE',  ( 0.000000000000000000, 0.000000000000000000, -1.000000000000000000 ) ) ;
#830 = CARTESIAN_POINT ( 'NONE',  ( 0.000000000000000000, 0.000000000000000000, 0.000000000000000000 ) ) ;
#831 = CARTESIAN_POINT ( 'NONE',  ( 0.000000000000000000, 54.20017844242556748, -32.11449294037138458 ) ) ;
#832 = CIRCLE ( 'NONE', #6896, 5.000000000000004441 ) ;
#833 = VERTEX_POINT ( 'NONE', #8602 ) ;
#834 = ORIENTED_EDGE ( 'NONE', *, *, #10294, .F. ) ;
#835 = AXIS2_PLACEMENT_3D ( 'NONE', #1508, #11788, #18648 ) ;
#836 = DIRECTION ( 'NONE',  ( 0.9995004958639132076, 0.000000000000000000, 0.03160314490350067673 ) ) ;
#837 = AXIS2_PLACEMENT_3D ( 'NONE', #16398, #9235, #12097 ) ;
#838 = ORIENTED_EDGE ( 'NONE', *, *, #5277, .F. ) ;
#839 = CARTESIAN_POINT ( 'NONE',  ( -2.500000000000000888, 0.000000000000000000, -4.974599999999998801 ) ) ;
#840 = CIRCLE ( 'NONE', #16638, 2.396904916527699214 ) ;
#841 = AXIS2_PLACEMENT_3D ( 'NONE', #6851, #12669, #4200 ) ;
#842 = CARTESIAN_POINT ( 'NONE',  ( -290.0000000000001137, -34.99999999999999289, -125.0000000000000000 ) ) ;
#843 = CIRCLE ( 'NONE', #12385, 1.249999999999999778 ) ;
#844 = DIRECTION ( 'NONE',  ( -1.000000000000000000, 0.000000000000000000, -0.000000000000000000 ) ) ;
#845 = VERTEX_POINT ( 'NONE', #8239 ) ;
#846 = AXIS2_PLACEMENT_3D ( 'NONE', #6460, #16655, #9411 ) ;
#847 = AXIS2_PLACEMENT_3D ( 'NONE', #1102, #721, #15482 ) ;
#848 = ORIENTED_EDGE ( 'NONE', *, *, #17503, .T. ) ;
#849 = DIRECTION ( 'NONE',  ( 0.000000000000000000, 0.000000000000000000, 1.000000000000000000 ) ) ;
#850 = CIRCLE ( 'NONE', #13002, 12.00000000001200462 ) ;
#851 = DIRECTION ( 'NONE',  ( -1.000000000000000000, 0.000000000000000000, 0.000000000000000000 ) ) ;
#852 = DIRECTION ( 'NONE',  ( 0.000000000000000000, 0.000000000000000000, -1.000000000000000000 ) ) ;
#853 = ORIENTED_EDGE ( 'NONE', *, *, #2346, .T. ) ;
#854 = DIRECTION ( 'NONE',  ( 0.000000000000000000, 0.000000000000000000, 1.000000000000000000 ) ) ;
#855 = ORIENTED_EDGE ( 'NONE', *, *, #1389, .F. ) ;
#856 = FACE_OUTER_BOUND ( 'NONE', #1144, .T. ) ;
#857 = CARTESIAN_POINT ( 'NONE',  ( -17.77999999999999758, 0.000000000000000000, 0.000000000000000000 ) ) ;
#858 = VERTEX_POINT ( 'NONE', #12806 ) ;
#859 = ORIENTED_EDGE ( 'NONE', *, *, #4333, .F. ) ;
#860 = FILL_AREA_STYLE ('',( #17053 ) ) ;
#861 = ORIENTED_EDGE ( 'NONE', *, *, #11844, .T. ) ;
#862 = CARTESIAN_POINT ( 'NONE',  ( -31.74999999999995737, 0.000000000000000000, 0.000000000000000000 ) ) ;
#863 = CARTESIAN_POINT ( 'NONE',  ( -11.25000000000000355, 0.000000000000000000, 0.000000000000000000 ) ) ;
#864 = AXIS2_PLACEMENT_3D ( 'NONE', #16750, #15599, #6828 ) ;
#865 = EDGE_CURVE ( 'NONE', #2263, #4026, #17287, .T. ) ;
#866 = ADVANCED_FACE ( 'NONE', ( #11278 ), #4139, .T. ) ;
#867 = CIRCLE ( 'NONE', #8153, 4.349594641156947716 ) ;
#868 = EDGE_CURVE ( 'NONE', #8500, #11257, #8513, .T. ) ;
#869 = CIRCLE ( 'NONE', #10578, 24.00000000002400213 ) ;
#870 = AXIS2_PLACEMENT_3D ( 'NONE', #15554, #18308, #10969 ) ;
#871 = ADVANCED_FACE ( 'NONE', ( #10038 ), #1003, .T. ) ;
#872 = VERTEX_POINT ( 'NONE', #17186 ) ;
#873 = VECTOR ( 'NONE', #3004, 1000.000000000000000 ) ;
#874 = ORIENTED_EDGE ( 'NONE', *, *, #16459, .T. ) ;
#875 = DIRECTION ( 'NONE',  ( 0.000000000000000000, 0.5877852522924742473, -0.8090169943749465631 ) ) ;
#876 = DIRECTION ( 'NONE',  ( -1.000000000000000000, -0.000000000000000000, -0.000000000000000000 ) ) ;
#877 = DIRECTION ( 'NONE',  ( 1.000000000000000000, 0.000000000000000000, 0.000000000000000000 ) ) ;
#878 = CARTESIAN_POINT ( 'NONE',  ( 0.000000000000000000, 34.13306034420185853, 44.70888270294173594 ) ) ;
#879 = AXIS2_PLACEMENT_3D ( 'NONE', #17078, #7057, #1436 ) ;
#880 = EDGE_CURVE ( 'NONE', #14362, #3677, #9321, .T. ) ;
#881 = DIRECTION ( 'NONE',  ( 0.000000000000000000, 0.000000000000000000, 1.000000000000000000 ) ) ;
#882 = COLOUR_RGB ( '',1.000000000000000000, 0.9490196078431372140, 0.9098039215686274384 ) ;
#883 = DIRECTION ( 'NONE',  ( 1.000000000000000000, -0.000000000000000000, -0.000000000000000000 ) ) ;
#884 = ORIENTED_EDGE ( 'NONE', *, *, #8191, .T. ) ;
#885 = AXIS2_PLACEMENT_3D ( 'NONE', #11911, #4767, #7626 ) ;
#886 = CARTESIAN_POINT ( 'NONE',  ( -90.70833251482494575, 2.081668171172168513E-14, -4.949572208642815774 ) ) ;
#887 = DIRECTION ( 'NONE',  ( 1.000000000000000000, 0.000000000000000000, 0.000000000000000000 ) ) ;
#888 = CARTESIAN_POINT ( 'NONE',  ( 0.000000000000000000, -39.14194549634393638, 40.58063702438330722 ) ) ;
#889 = EDGE_CURVE ( 'NONE', #4270, #8736, #1731, .T. ) ;
#890 = VERTEX_POINT ( 'NONE', #2425 ) ;
#891 = VECTOR ( 'NONE', #1458, 1000.000000000000000 ) ;
#892 = CIRCLE ( 'NONE', #4521, 2.649999999999992806 ) ;
#893 = ORIENTED_EDGE ( 'NONE', *, *, #17398, .F. ) ;
#894 = CIRCLE ( 'NONE', #765, 63.00000000006298961 ) ;
#895 = AXIS2_PLACEMENT_3D ( 'NONE', #12553, #12357, #2264 ) ;
#896 = EDGE_CURVE ( 'NONE', #9406, #17827, #5654, .T. ) ;
#897 = ORIENTED_EDGE ( 'NONE', *, *, #12369, .F. ) ;
#898 = CARTESIAN_POINT ( 'NONE',  ( 13.90576474687263264, 0.000000000000000000, -42.79754323328189969 ) ) ;
#899 = FACE_OUTER_BOUND ( 'NONE', #8207, .T. ) ;
#900 = CARTESIAN_POINT ( 'NONE',  ( 0.000000000000000000, 0.000000000000000000, -4.974599999999998801 ) ) ;
#901 = FACE_OUTER_BOUND ( 'NONE', #11513, .T. ) ;
#902 = CYLINDRICAL_SURFACE ( 'NONE', #8214, 63.00000000006298961 ) ;
#903 = DIRECTION ( 'NONE',  ( 0.000000000000000000, 0.000000000000000000, 1.000000000000000000 ) ) ;
#904 = DIRECTION ( 'NONE',  ( 0.9995004958639132076, 0.000000000000000000, 0.03160314490350067673 ) ) ;
#905 = DIRECTION ( 'NONE',  ( 0.000000000000000000, 0.000000000000000000, 1.000000000000000000 ) ) ;
#906 = VERTEX_POINT ( 'NONE', #8420 ) ;
#907 = DIRECTION ( 'NONE',  ( 1.000000000000000000, 0.000000000000000000, 0.000000000000000000 ) ) ;
#908 = ORIENTED_EDGE ( 'NONE', *, *, #630, .T. ) ;
#909 = VECTOR ( 'NONE', #15611, 1000.000000000000000 ) ;
#910 = CARTESIAN_POINT ( 'NONE',  ( 0.2500000000000002220, 0.000000000000000000, 4.000000000000000000 ) ) ;
#911 = CARTESIAN_POINT ( 'NONE',  ( 0.000000000000000000, -17.25000000000000355, 0.000000000000000000 ) ) ;
#912 = VERTEX_POINT ( 'NONE', #14328 ) ;
#913 = ORIENTED_EDGE ( 'NONE', *, *, #375, .F. ) ;
#914 = CARTESIAN_POINT ( 'NONE',  ( 10.00000000000000000, 0.000000000000000000, 0.000000000000000000 ) ) ;
#915 = DIRECTION ( 'NONE',  ( 0.000000000000000000, 0.000000000000000000, 1.000000000000000000 ) ) ;
#916 = ORIENTED_EDGE ( 'NONE', *, *, #16337, .F. ) ;
#917 = EDGE_CURVE ( 'NONE', #6918, #17767, #10543, .T. ) ;
#918 = AXIS2_PLACEMENT_3D ( 'NONE', #739, #8350, #13974 ) ;
#919 = FACE_OUTER_BOUND ( 'NONE', #1318, .T. ) ;
#920 = CARTESIAN_POINT ( 'NONE',  ( 0.000000000000000000, 55.74967257055882186, 7.478235706489174461 ) ) ;
#921 = DIRECTION ( 'NONE',  ( 0.000000000000000000, 0.000000000000000000, -1.000000000000000000 ) ) ;
#922 = CARTESIAN_POINT ( 'NONE',  ( 4.000000000000000000, 2.309401076758497151, -3.433295621305379353 ) ) ;
#923 = VERTEX_POINT ( 'NONE', #15566 ) ;
#924 = CARTESIAN_POINT ( 'NONE',  ( 2.500000000000000000, -2.357898499370432166, 3.035766082959412415E-15 ) ) ;
#925 = ORIENTED_EDGE ( 'NONE', *, *, #7615, .T. ) ;
#926 = CARTESIAN_POINT ( 'NONE',  ( 0.6448876103708359731, 4.246476118072354922, -0.2256878752776725616 ) ) ;
#927 = LINE ( 'NONE', #5287, #18650 ) ;
#929 = AXIS2_PLACEMENT_3D ( 'NONE', #6910, #2336, #1890 ) ;
#928 = CARTESIAN_POINT ( 'NONE',  ( 10.00000000000000000, -27.72801475327278453, -5.086963483077506787 ) ) ;
#930 = ORIENTED_EDGE ( 'NONE', *, *, #7358, .T. ) ;
#931 = VERTEX_POINT ( 'NONE', #2514 ) ;
#932 = PLANE ( 'NONE',  #17225 ) ;
#933 = AXIS2_PLACEMENT_3D ( 'NONE', #17379, #1641, #13097 ) ;
#934 =( LENGTH_UNIT ( ) NAMED_UNIT ( * ) SI_UNIT ( .MILLI., .METRE. ) );
#935 = EDGE_CURVE ( 'NONE', #12093, #13795, #11151, .T. ) ;
#936 = ORIENTED_EDGE ( 'NONE', *, *, #11799, .F. ) ;
#937 = CARTESIAN_POINT ( 'NONE',  ( -10.00000000000000000, 0.000000000000000000, 0.000000000000000000 ) ) ;
#938 = EDGE_CURVE ( 'NONE', #1081, #872, #7506, .T. ) ;
#939 = LINE ( 'NONE', #5113, #18715 ) ;
#940 = DIRECTION ( 'NONE',  ( 0.000000000000000000, 0.000000000000000000, 1.000000000000000000 ) ) ;
#941 = VERTEX_POINT ( 'NONE', #5479 ) ;
#943 = CIRCLE ( 'NONE', #1542, 30.00000000000000000 ) ;
#942 = DIRECTION ( 'NONE',  ( -1.000000000000000000, 0.000000000000000000, 0.000000000000000000 ) ) ;
#944 = VERTEX_POINT ( 'NONE', #4050 ) ;
#945 = CARTESIAN_POINT ( 'NONE',  ( 4.175002511812151873, 2.208363329454889445, -3.469254087858244073 ) ) ;
#946 = FACE_OUTER_BOUND ( 'NONE', #13197, .T. ) ;
#947 = CARTESIAN_POINT ( 'NONE',  ( 0.000000000000000000, 5.940243314904670946, -32.46095361140686464 ) ) ;
#948 = ORIENTED_EDGE ( 'NONE', *, *, #9136, .F. ) ;
#949 = CARTESIAN_POINT ( 'NONE',  ( -90.00000000009001155, -10.00000000000001599, -1.301042606982603940E-15 ) ) ;
#950 = ORIENTED_EDGE ( 'NONE', *, *, #13546, .T. ) ;
#951 = CARTESIAN_POINT ( 'NONE',  ( 0.000000000000000000, -38.81885513159959800, -40.70683587897998734 ) ) ;
#952 = DIRECTION ( 'NONE',  ( -1.000000000000000000, 0.000000000000000000, 0.000000000000000000 ) ) ;
#953 = EDGE_LOOP ( 'NONE', ( #7629, #7949, #7760, #5155 ) ) ;
#954 = ORIENTED_EDGE ( 'NONE', *, *, #16912, .F. ) ;
#955 = ORIENTED_EDGE ( 'NONE', *, *, #4704, .T. ) ;
#956 = CYLINDRICAL_SURFACE ( 'NONE', #8481, 2.649999999999992806 ) ;
#957 = CARTESIAN_POINT ( 'NONE',  ( 0.000000000000000000, -15.61693798565540625, 61.03368945066429774 ) ) ;
#958 = EDGE_LOOP ( 'NONE', ( #6895, #6148, #2898, #7199 ) ) ;
#959 = EDGE_LOOP ( 'NONE', ( #11211, #1552, #16308, #16327 ) ) ;
#960 = DIRECTION ( 'NONE',  ( 0.000000000000000000, -1.000000000000000000, 0.000000000000000000 ) ) ;
#961 = CARTESIAN_POINT ( 'NONE',  ( 4.000000000000000000, -2.309401076758516691, -0.4999999999999995559 ) ) ;
#962 = CARTESIAN_POINT ( 'NONE',  ( 8.673617379884035472E-16, 4.618802153517012954, -5.000000000000000000 ) ) ;
#963 = CARTESIAN_POINT ( 'NONE',  ( 4.144923636027600722, -29.35885059145708098, 0.000000000000000000 ) ) ;
#964 = EDGE_CURVE ( 'NONE', #15321, #11704, #17262, .T. ) ;
#965 = AXIS2_PLACEMENT_3D ( 'NONE', #3766, #2330, #12151 ) ;
#966 = EDGE_CURVE ( 'NONE', #7707, #2762, #16570, .T. ) ;
#967 = CARTESIAN_POINT ( 'NONE',  ( 13.90576474687263264, 0.000000000000000000, -40.14754323328190111 ) ) ;
#968 = CARTESIAN_POINT ( 'NONE',  ( 0.000000000000000000, 42.79754323328179311, -11.25576474687299644 ) ) ;
#969 = CARTESIAN_POINT ( 'NONE',  ( 2.500000000000000000, 0.000000000000000000, 0.000000000000000000 ) ) ;
#970 = ORIENTED_EDGE ( 'NONE', *, *, #12368, .T. ) ;
#971 = CARTESIAN_POINT ( 'NONE',  ( 10.00000000000000000, 15.61693798565496749, 61.03368945066440432 ) ) ;
#972 = CARTESIAN_POINT ( 'NONE',  ( 10.00000000000000000, 1.489278925039520418, 26.20671763660628883 ) ) ;
#973 = AXIS2_PLACEMENT_3D ( 'NONE', #2003, #13534, #482 ) ;
#974 = CARTESIAN_POINT ( 'NONE',  ( 2.000000000000000000, -6.429618962271402616, 0.000000000000000000 ) ) ;
#975 = DIRECTION ( 'NONE',  ( -1.000000000000000000, -0.000000000000000000, 0.000000000000000000 ) ) ;
#976 = EDGE_CURVE ( 'NONE', #6348, #14291, #9950, .T. ) ;
#977 = ORIENTED_EDGE ( 'NONE', *, *, #6473, .T. ) ;
#978 = ORIENTED_EDGE ( 'NONE', *, *, #14408, .T. ) ;
#979 = ADVANCED_FACE ( 'NONE', ( #674 ), #9325, .F. ) ;
#980 = VERTEX_POINT ( 'NONE', #11039 ) ;
#982 = CARTESIAN_POINT ( 'NONE',  ( 0.000000000000000000, 10.00000000000000000, -30.00000000000000000 ) ) ;
#981 = AXIS2_PLACEMENT_3D ( 'NONE', #2769, #16864, #12672 ) ;
#983 = CARTESIAN_POINT ( 'NONE',  ( 10.00000000000000000, 0.000000000000000000, 0.000000000000000000 ) ) ;
#984 = CARTESIAN_POINT ( 'NONE',  ( 10.00000000000000000, 0.000000000000000000, 0.000000000000000000 ) ) ;
#985 = DIRECTION ( 'NONE',  ( -1.000000000000000000, 0.000000000000000000, -0.000000000000000000 ) ) ;
#986 = EDGE_CURVE ( 'NONE', #1108, #15167, #9015, .T. ) ;
#987 = LINE ( 'NONE', #4467, #16642 ) ;
#988 = ADVANCED_FACE ( 'NONE', ( #14004, #12479 ), #3723, .T. ) ;
#989 = CARTESIAN_POINT ( 'NONE',  ( 0.000000000000000000, 48.50907078259439942, -40.19788616105557111 ) ) ;
#990 = LINE ( 'NONE', #1078, #10722 ) ;
#991 = DIRECTION ( 'NONE',  ( 0.000000000000000000, 0.000000000000000000, 1.000000000000000000 ) ) ;
#992 = ORIENTED_EDGE ( 'NONE', *, *, #12234, .T. ) ;
#993 = DIRECTION ( 'NONE',  ( -1.000000000000000000, 0.000000000000000000, -0.000000000000000000 ) ) ;
#994 = ORIENTED_EDGE ( 'NONE', *, *, #375, .T. ) ;
#995 = AXIS2_PLACEMENT_3D ( 'NONE', #17671, #3385, #1944 ) ;
#996 = EDGE_CURVE ( 'NONE', #8916, #9803, #18000, .T. ) ;
#997 = DIRECTION ( 'NONE',  ( 1.000000000000000000, 0.000000000000000000, 0.000000000000000000 ) ) ;
#998 = DIRECTION ( 'NONE',  ( 0.000000000000000000, 1.000000000000000000, 0.000000000000000000 ) ) ;
#999 = ORIENTED_EDGE ( 'NONE', *, *, #11126, .T. ) ;
#1000 = ORIENTED_EDGE ( 'NONE', *, *, #7256, .T. ) ;
#1001 = EDGE_CURVE ( 'NONE', #1864, #17712, #2279, .T. ) ;
#1002 = CARTESIAN_POINT ( 'NONE',  ( -3.349226789952655547, -2.685125164760744809, -0.2236248678334863682 ) ) ;
#1003 = CYLINDRICAL_SURFACE ( 'NONE', #14209, 56.24900000005625600 ) ;
#1004 = ORIENTED_EDGE ( 'NONE', *, *, #9404, .T. ) ;
#1005 = DIRECTION ( 'NONE',  ( 0.000000000000000000, 0.000000000000000000, 1.000000000000000000 ) ) ;
#1006 = CARTESIAN_POINT ( 'NONE',  ( -117.1020693116506379, -30.00000000000000000, -19.69080595179801207 ) ) ;
#1007 = CARTESIAN_POINT ( 'NONE',  ( 10.00000000000000000, 0.000000000000000000, 0.000000000000000000 ) ) ;
#1008 = CARTESIAN_POINT ( 'NONE',  ( 32.50000000000000000, -30.00000000000000000, 3.680389326632394941E-13 ) ) ;
#1009 = CIRCLE ( 'NONE', #13174, 2.649999999999999467 ) ;
#1010 = CIRCLE ( 'NONE', #18331, 63.00000000006298961 ) ;
#1011 = CLOSED_SHELL ( 'NONE', ( #7441, #11689, #11568, #2661, #16694, #4242, #6924, #17624, #7600, #3905, #9825, #4801, #9295, #17673, #7168, #6200, #11234, #2883, #16242, #7379, #4112, #1234, #14456, #2013, #11918, #5051, #647, #1767, #1331, #17222, #4597, #7891, #15182 ) ) ;
#1012 = DIRECTION ( 'NONE',  ( 0.000000000000000000, 0.4999999999999990008, -0.8660254037844391517 ) ) ;
#1013 = ORIENTED_EDGE ( 'NONE', *, *, #9491, .T. ) ;
#1014 = CARTESIAN_POINT ( 'NONE',  ( 0.000000000000000000, 0.000000000000000000, 0.000000000000000000 ) ) ;
#1015 = DIRECTION ( 'NONE',  ( 0.000000000000000000, -1.000000000000000000, 0.000000000000000000 ) ) ;
#1016 = CARTESIAN_POINT ( 'NONE',  ( 0.000000000000000000, 0.000000000000000000, -5.000000000000000000 ) ) ;
#1017 = ORIENTED_EDGE ( 'NONE', *, *, #815, .T. ) ;
#1018 = VERTEX_POINT ( 'NONE', #15155 ) ;
#1019 = EDGE_CURVE ( 'NONE', #13886, #4065, #8289, .T. ) ;
#1020 = CARTESIAN_POINT ( 'NONE',  ( -56.50000000009000445, -34.99999999999999289, -2.649999999999610889 ) ) ;
#1021 = SHAPE_REPRESENTATION_RELATIONSHIP ( 'NONE' , 'NONE' ,  #8256, #4884 ) ;
#1022 = ORIENTED_EDGE ( 'NONE', *, *, #2377, .T. ) ;
#1023 = DIRECTION ( 'NONE',  ( 0.000000000000000000, 0.000000000000000000, 1.000000000000000000 ) ) ;
#1024 = CIRCLE ( 'NONE', #4368, 25.00000000000000000 ) ;
#1025 = DIRECTION ( 'NONE',  ( -1.000000000000000000, -0.000000000000000000, -0.000000000000000000 ) ) ;
#1026 = DIRECTION ( 'NONE',  ( -1.000000000000000000, 0.000000000000000000, -0.000000000000000000 ) ) ;
#1027 = ORIENTED_EDGE ( 'NONE', *, *, #8334, .T. ) ;
#1028 = DIRECTION ( 'NONE',  ( -1.000000000000000000, -0.000000000000000000, -0.000000000000000000 ) ) ;
#1029 = EDGE_LOOP ( 'NONE', ( #970, #3446 ) ) ;
#1031 = CARTESIAN_POINT ( 'NONE',  ( -0.02511973781850462134, 4.877415612947412882, -3.751298745799839462 ) ) ;
#1030 = UNCERTAINTY_MEASURE_WITH_UNIT (LENGTH_MEASURE( 1.000000000000000082E-05 ), #12629, 'distance_accuracy_value', 'NONE');
#1032 = DIRECTION ( 'NONE',  ( 1.000000000000000000, -0.000000000000000000, 0.000000000000000000 ) ) ;
#1033 = DIRECTION ( 'NONE',  ( 0.000000000000000000, 0.000000000000000000, 1.000000000000000000 ) ) ;
#1034 = ORIENTED_EDGE ( 'NONE', *, *, #13070, .T. ) ;
#1035 = CARTESIAN_POINT ( 'NONE',  ( 2.500000000000000000, -1.178949249685214307, 2.042000000000001592 ) ) ;
#1036 = ORIENTED_EDGE ( 'NONE', *, *, #3420, .F. ) ;
#1037 = AXIS2_PLACEMENT_3D ( 'NONE', #6039, #12130, #16426 ) ;
#1038 = DIRECTION ( 'NONE',  ( 0.000000000000000000, 0.000000000000000000, 1.000000000000000000 ) ) ;
#1039 = FACE_OUTER_BOUND ( 'NONE', #2644, .T. ) ;
#1040 = ORIENTED_EDGE ( 'NONE', *, *, #746, .T. ) ;
#1041 = ORIENTED_EDGE ( 'NONE', *, *, #1490, .T. ) ;
#1042 = EDGE_CURVE ( 'NONE', #14980, #3488, #16030, .T. ) ;
#1043 = CARTESIAN_POINT ( 'NONE',  ( 1.250000000000000000, -6.429618962271402616, -1.000000000000000000 ) ) ;
#1044 = ORIENTED_EDGE ( 'NONE', *, *, #4817, .F. ) ;
#1045 = DIRECTION ( 'NONE',  ( 0.000000000000000000, 0.000000000000000000, 1.000000000000000000 ) ) ;
#1046 = CARTESIAN_POINT ( 'NONE',  ( -79.64793068852927149, -34.99999999999999289, 29.21039329588765554 ) ) ;
#1047 = ADVANCED_FACE ( 'NONE', ( #3810 ), #12571, .T. ) ;
#1048 = ORIENTED_EDGE ( 'NONE', *, *, #7143, .T. ) ;
#1049 = ORIENTED_EDGE ( 'NONE', *, *, #1352, .T. ) ;
#1050 = CARTESIAN_POINT ( 'NONE',  ( 10.00000000000000000, -5.876895005582881026, 62.72529079327804169 ) ) ;
#1051 = CARTESIAN_POINT ( 'NONE',  ( -117.1020693116508085, -34.99999999999999289, 19.69080595179778115 ) ) ;
#1052 = CARTESIAN_POINT ( 'NONE',  ( 10.00000000000000000, -9.823366686500245137, -55.51919907100663920 ) ) ;
#1053 = FACE_BOUND ( 'NONE', #18533, .T. ) ;
#1054 = ADVANCED_FACE ( 'NONE', ( #18092 ), #18374, .T. ) ;
#1055 = DIRECTION ( 'NONE',  ( -1.000000000000000000, 0.000000000000000000, 0.000000000000000000 ) ) ;
#1056 = CARTESIAN_POINT ( 'NONE',  ( 2.500000000000000000, 0.000000000000000000, 0.000000000000000000 ) ) ;
#1057 = CARTESIAN_POINT ( 'NONE',  ( 0.000000000000000000, 20.41355805489615705, 19.44239304137382973 ) ) ;
#1058 = ORIENTED_EDGE ( 'NONE', *, *, #7053, .T. ) ;
#1059 = DIRECTION ( 'NONE',  ( 1.000000000000000000, 0.000000000000000000, 0.000000000000000000 ) ) ;
#1060 = CYLINDRICAL_SURFACE ( 'NONE', #7471, 63.00000000006298961 ) ;
#1061 =( GEOMETRIC_REPRESENTATION_CONTEXT ( 3 ) GLOBAL_UNCERTAINTY_ASSIGNED_CONTEXT ( ( #11305 ) ) GLOBAL_UNIT_ASSIGNED_CONTEXT ( ( #18056, #3403, #7766 ) ) REPRESENTATION_CONTEXT ( 'NONE', 'WORKASPACE' ) );
#1062 = DIRECTION ( 'NONE',  ( 1.000000000000000000, 0.000000000000000000, 0.000000000000000000 ) ) ;
#1063 = DIRECTION ( 'NONE',  ( -1.000000000000000000, -0.000000000000000000, 0.000000000000000000 ) ) ;
#1064 = AXIS2_PLACEMENT_3D ( 'NONE', #13787, #851, #4931 ) ;
#1065 = EDGE_LOOP ( 'NONE', ( #3298, #16949, #2745, #15966 ) ) ;
#1066 = EDGE_CURVE ( 'NONE', #16979, #9984, #13601, .T. ) ;
#1067 = EDGE_LOOP ( 'NONE', ( #18299, #7502, #7090, #2569 ) ) ;
#1068 = EDGE_LOOP ( 'NONE', ( #4777, #8665 ) ) ;
#1069 =( GEOMETRIC_REPRESENTATION_CONTEXT ( 3 ) GLOBAL_UNCERTAINTY_ASSIGNED_CONTEXT ( ( #5594 ) ) GLOBAL_UNIT_ASSIGNED_CONTEXT ( ( #8899, #15869, #7467 ) ) REPRESENTATION_CONTEXT ( 'NONE', 'WORKASPACE' ) );
#1070 = CARTESIAN_POINT ( 'NONE',  ( -36.40576474687271258, 10.00000000000000000, -26.45033635316118747 ) ) ;
#1071 = CYLINDRICAL_SURFACE ( 'NONE', #11264, 25.00000000000000000 ) ;
#1072 = CIRCLE ( 'NONE', #13240, 12.00000000001200462 ) ;
#1073 = DIRECTION ( 'NONE',  ( -1.000000000000000000, 0.000000000000000000, 0.000000000000000000 ) ) ;
#1074 = AXIS2_PLACEMENT_3D ( 'NONE', #18222, #3466, #9453 ) ;
#1075 = DIRECTION ( 'NONE',  ( -2.031314180040284764E-16, -1.000000000000000000, -1.301042606982601377E-16 ) ) ;
#1076 = CARTESIAN_POINT ( 'NONE',  ( 50.00005079999999680, 6.799999999999999822, 1.500000000000000000 ) ) ;
#1077 = FACE_OUTER_BOUND ( 'NONE', #3375, .T. ) ;
#1078 = CARTESIAN_POINT ( 'NONE',  ( -90.00000000009001155, -49.14213562373095812, -5.000000000000005329 ) ) ;
#1079 = DIRECTION ( 'NONE',  ( -0.000000000000000000, 1.000000000000000000, -0.000000000000000000 ) ) ;
#1080 = ADVANCED_FACE ( 'NONE', ( #15331 ), #7997, .T. ) ;
#1081 = VERTEX_POINT ( 'NONE', #13808 ) ;
#1082 = CARTESIAN_POINT ( 'NONE',  ( 10.00000000000000000, 0.000000000000000000, 0.000000000000000000 ) ) ;
#1083 = ORIENTED_EDGE ( 'NONE', *, *, #7405, .T. ) ;
#1084 = CARTESIAN_POINT ( 'NONE',  ( 10.00000000000000000, 0.000000000000000000, 0.000000000000000000 ) ) ;
#1085 = CARTESIAN_POINT ( 'NONE',  ( 10.00000000000000000, 57.83923611457354497, -24.97244012287440640 ) ) ;
#1086 = EDGE_LOOP ( 'NONE', ( #17308, #8677, #4999, #18206 ) ) ;
#1087 = CARTESIAN_POINT ( 'NONE',  ( -90.00000000009001155, -34.99999999999999289, -1.301042606982605321E-15 ) ) ;
#1088 = CARTESIAN_POINT ( 'NONE',  ( -79.64793068852925728, -43.00000000000000000, 31.86039329588764701 ) ) ;
#1089 = ORIENTED_EDGE ( 'NONE', *, *, #8610, .F. ) ;
#1090 = DIRECTION ( 'NONE',  ( 1.000000000000000000, 0.000000000000000000, 0.000000000000000000 ) ) ;
#1091 = VERTEX_POINT ( 'NONE', #771 ) ;
#1092 = AXIS2_PLACEMENT_3D ( 'NONE', #3107, #3481, #15008 ) ;
#1093 = AXIS2_PLACEMENT_3D ( 'NONE', #13536, #6293, #8000 ) ;
#1094 = EDGE_CURVE ( 'NONE', #9382, #7210, #11467, .T. ) ;
#1095 = ADVANCED_FACE ( 'NONE', ( #18192 ), #16772, .F. ) ;
#1096 = ADVANCED_FACE ( 'NONE', ( #13912 ), #13894, .T. ) ;
#1097 = CYLINDRICAL_SURFACE ( 'NONE', #11726, 12.00000000001200462 ) ;
#1098 = EDGE_CURVE ( 'NONE', #9858, #9496, #5683, .T. ) ;
#1099 = DIRECTION ( 'NONE',  ( -1.000000000000000000, 0.000000000000000000, 0.000000000000000000 ) ) ;
#1100 = CIRCLE ( 'NONE', #7769, 63.00000000006298961 ) ;
#1101 = CIRCLE ( 'NONE', #800, 2.500000000000000888 ) ;
#1102 = CARTESIAN_POINT ( 'NONE',  ( 2.500000000000000000, 2.357898499370432166, -2.385244779468109755E-15 ) ) ;
#1103 = CARTESIAN_POINT ( 'NONE',  ( 2.500000000000000000, -2.357898499370432166, 3.035766082959412415E-15 ) ) ;
#1104 = EDGE_CURVE ( 'NONE', #5754, #8001, #16320, .T. ) ;
#1105 = AXIS2_PLACEMENT_3D ( 'NONE', #4053, #17378, #12810 ) ;
#1106 = CARTESIAN_POINT ( 'NONE',  ( -11.15000000000000391, 0.000000000000000000, 0.000000000000000000 ) ) ;
#1107 = AXIS2_PLACEMENT_3D ( 'NONE', #18507, #18599, #1363 ) ;
#1108 = VERTEX_POINT ( 'NONE', #12950 ) ;
#1109 = EDGE_CURVE ( 'NONE', #8874, #6557, #18464, .T. ) ;
#1110 = DIRECTION ( 'NONE',  ( 1.000000000000000000, -3.469446951953611231E-16, 0.000000000000000000 ) ) ;
#1111 = CARTESIAN_POINT ( 'NONE',  ( 0.000000000000000000, -24.33982105418865061, -50.71018745830470920 ) ) ;
#1112 = DIRECTION ( 'NONE',  ( 1.000000000000000000, -0.000000000000000000, -0.000000000000000000 ) ) ;
#1113 = ORIENTED_EDGE ( 'NONE', *, *, #7721, .T. ) ;
#1114 = ORIENTED_EDGE ( 'NONE', *, *, #90, .F. ) ;
#1115 = APPLICATION_CONTEXT ( 'automotive_design' ) ;
#1116 = CARTESIAN_POINT ( 'NONE',  ( 0.000000000000000000, -24.68609584167124282, -50.69000562871667626 ) ) ;
#1117 = ORIENTED_EDGE ( 'NONE', *, *, #2996, .T. ) ;
#1118 = CARTESIAN_POINT ( 'NONE',  ( 10.00000000000000000, 16.60877409751197575, -20.32630374611166957 ) ) ;
#1119 = AXIS2_PLACEMENT_3D ( 'NONE', #4299, #11626, #1616 ) ;
#1120 = EDGE_CURVE ( 'NONE', #3525, #5795, #18757, .T. ) ;
#1121 = AXIS2_PLACEMENT_3D ( 'NONE', #7531, #10470, #14766 ) ;
#1122 = AXIS2_PLACEMENT_3D ( 'NONE', #9107, #3209, #11872 ) ;
#1123 = DIRECTION ( 'NONE',  ( 0.000000000000000000, 1.000000000000000000, 0.000000000000000000 ) ) ;
#1124 = DIRECTION ( 'NONE',  ( -1.000000000000000000, -0.000000000000000000, -0.000000000000000000 ) ) ;
#1125 = ADVANCED_FACE ( 'NONE', ( #8381 ), #5532, .F. ) ;
#1126 = EDGE_LOOP ( 'NONE', ( #813, #5939 ) ) ;
#1127 = DIRECTION ( 'NONE',  ( -0.000000000000000000, 1.000000000000000000, 0.000000000000000000 ) ) ;
#1128 = EDGE_LOOP ( 'NONE', ( #12006, #3381, #1622, #7072 ) ) ;
#1129 = CARTESIAN_POINT ( 'NONE',  ( 10.00000000000000000, -61.03368945066446116, 15.61693798565474012 ) ) ;
#1130 = DIRECTION ( 'NONE',  ( -1.000000000000000000, -0.000000000000000000, 0.000000000000000000 ) ) ;
#1132 = CIRCLE ( 'NONE', #8970, 24.00000000002400213 ) ;
#1131 = PLANE ( 'NONE',  #4489 ) ;
#1133 = EDGE_LOOP ( 'NONE', ( #14796, #17474, #167, #6880 ) ) ;
#1134 = CARTESIAN_POINT ( 'NONE',  ( 0.000000000000000000, 15.68049343256038064, -29.03656532225546627 ) ) ;
#1135 = ORIENTED_EDGE ( 'NONE', *, *, #868, .T. ) ;
#1136 = VECTOR ( 'NONE', #675, 1000.000000000000000 ) ;
#1137 = DIRECTION ( 'NONE',  ( -1.000000000000000000, 2.312964634635740492E-16, 0.000000000000000000 ) ) ;
#1138 = CYLINDRICAL_SURFACE ( 'NONE', #11634, 56.24900000005625600 ) ;
#1139 = CIRCLE ( 'NONE', #8731, 56.24900000005626310 ) ;
#1140 = ORIENTED_EDGE ( 'NONE', *, *, #865, .F. ) ;
#1141 = ORIENTED_EDGE ( 'NONE', *, *, #12608, .F. ) ;
#1142 = AXIS2_PLACEMENT_3D ( 'NONE', #6761, #12283, #583 ) ;
#1143 = DIRECTION ( 'NONE',  ( -1.000000000000000000, 0.000000000000000000, 0.000000000000000000 ) ) ;
#1144 = EDGE_LOOP ( 'NONE', ( #12663, #16681, #4780, #9245 ) ) ;
#1145 = DIRECTION ( 'NONE',  ( 0.000000000000000000, 0.000000000000000000, 1.000000000000000000 ) ) ;
#1146 = DIRECTION ( 'NONE',  ( 0.000000000000000000, -0.4539904997395351471, -0.8910065241883737830 ) ) ;
#1147 = CIRCLE ( 'NONE', #223, 12.00000000001200107 ) ;
#1148 = VECTOR ( 'NONE', #18172, 1000.000000000000000 ) ;
#1149 = VECTOR ( 'NONE', #3764, 1000.000000000000000 ) ;
#1150 = VECTOR ( 'NONE', #4790, 1000.000000000000000 ) ;
#1151 = EDGE_CURVE ( 'NONE', #6853, #4502, #11242, .T. ) ;
#1152 = VERTEX_POINT ( 'NONE', #10180 ) ;
#1153 = ORIENTED_EDGE ( 'NONE', *, *, #976, .T. ) ;
#1154 = DIRECTION ( 'NONE',  ( -1.000000000000000000, -0.000000000000000000, 0.000000000000000000 ) ) ;
#1155 = CARTESIAN_POINT ( 'NONE',  ( -1.391697335622809950, -4.043246145443391448, -3.503898532754372575 ) ) ;
#1156 = CARTESIAN_POINT ( 'NONE',  ( 0.000000000000000000, 0.000000000000000000, -2.000000000000000000 ) ) ;
#1157 = DIRECTION ( 'NONE',  ( -1.000000000000000000, 0.000000000000000000, 0.000000000000000000 ) ) ;
#1158 = CARTESIAN_POINT ( 'NONE',  ( 10.00000000000000000, 45.00825343885067298, -33.95787273855199828 ) ) ;
#1159 = CARTESIAN_POINT ( 'NONE',  ( -26.29305231718568336, -34.99999999999999289, -19.10302069950552095 ) ) ;
#1160 = CONICAL_SURFACE ( 'NONE', #12711, 4.000000000000000000, 0.8911886515913786111 ) ;
#1161 = PLANE ( 'NONE',  #8704 ) ;
#1162 = VERTEX_POINT ( 'NONE', #5716 ) ;
#1163 = DIRECTION ( 'NONE',  ( 0.9995004958639132076, 0.000000000000000000, 0.03160314490350067673 ) ) ;
#1164 = DIRECTION ( 'NONE',  ( -1.000000000000000000, 0.000000000000000000, 0.000000000000000000 ) ) ;
#1165 = CIRCLE ( 'NONE', #4494, 2.649999999999992806 ) ;
#1166 = DIRECTION ( 'NONE',  ( 0.000000000000000000, 0.000000000000000000, 1.000000000000000000 ) ) ;
#1167 = DIRECTION ( 'NONE',  ( 0.000000000000000000, 1.000000000000000000, 0.000000000000000000 ) ) ;
#1168 = AXIS2_PLACEMENT_3D ( 'NONE', #4885, #17740, #6311 ) ;
#1169 = VECTOR ( 'NONE', #13558, 1000.000000000000114 ) ;
#1170 = EDGE_CURVE ( 'NONE', #7123, #7186, #9632, .T. ) ;
#1171 = VERTEX_POINT ( 'NONE', #5806 ) ;
#1172 = EDGE_CURVE ( 'NONE', #8441, #9928, #14502, .T. ) ;
#1173 = CIRCLE ( 'NONE', #2073, 2.041999999999999815 ) ;
#1174 = ORIENTED_EDGE ( 'NONE', *, *, #18088, .F. ) ;
#1175 = DIRECTION ( 'NONE',  ( 0.000000000000000000, 0.000000000000000000, 1.000000000000000000 ) ) ;
#1176 = FILL_AREA_STYLE_COLOUR ( '', #11588 ) ;
#1177 = CIRCLE ( 'NONE', #14554, 24.00000000002400213 ) ;
#1178 = VERTEX_POINT ( 'NONE', #8655 ) ;
#1179 = CIRCLE ( 'NONE', #4510, 30.00000000000000711 ) ;
#1180 =( LENGTH_UNIT ( ) NAMED_UNIT ( * ) SI_UNIT ( .MILLI., .METRE. ) );
#1181 = CARTESIAN_POINT ( 'NONE',  ( 0.000000000000000000, -41.62350880771888484, -47.29147401531999861 ) ) ;
#1182 = LINE ( 'NONE', #4037, #9056 ) ;
#1183 = DIRECTION ( 'NONE',  ( 0.000000000000000000, -6.982962677686266711E-15, 1.000000000000000000 ) ) ;
#1184 = DIRECTION ( 'NONE',  ( 0.000000000000000000, 0.000000000000000000, 1.000000000000000000 ) ) ;
#1185 = ORIENTED_EDGE ( 'NONE', *, *, #8556, .F. ) ;
#1186 = CARTESIAN_POINT ( 'NONE',  ( -4.000000000000000888, 1.563622288139195238, -0.2253451193528307472 ) ) ;
#1187 = VERTEX_POINT ( 'NONE', #7045 ) ;
#1188 = FACE_OUTER_BOUND ( 'NONE', #17037, .T. ) ;
#1189 = ORIENTED_EDGE ( 'NONE', *, *, #10587, .T. ) ;
#1190 = DIRECTION ( 'NONE',  ( -0.5000000000000016653, 0.8660254037844378194, 0.000000000000000000 ) ) ;
#1191 = DIRECTION ( 'NONE',  ( -1.277094964440070034E-16, -1.000000000000000000, 4.444473246549030520E-17 ) ) ;
#1192 = CIRCLE ( 'NONE', #4821, 56.24900000005627021 ) ;
#1193 = DIRECTION ( 'NONE',  ( 0.000000000000000000, 0.000000000000000000, -1.000000000000000000 ) ) ;
#1194 = ORIENTED_EDGE ( 'NONE', *, *, #5338, .F. ) ;
#1195 = AXIS2_PLACEMENT_3D ( 'NONE', #7428, #1717, #9049 ) ;
#1196 = CIRCLE ( 'NONE', #11825, 33.00000000003299760 ) ;
#1197 = CARTESIAN_POINT ( 'NONE',  ( 0.000000000000000000, 0.000000000000000000, 0.000000000000000000 ) ) ;
#1198 = DIRECTION ( 'NONE',  ( 0.000000000000000000, 0.000000000000000000, 1.000000000000000000 ) ) ;
#1199 = VECTOR ( 'NONE', #14595, 1000.000000000000000 ) ;
#1200 = DIRECTION ( 'NONE',  ( 0.000000000000000000, 0.000000000000000000, 1.000000000000000000 ) ) ;
#1201 = DIRECTION ( 'NONE',  ( 1.000000000000000000, 0.000000000000000000, 0.000000000000000000 ) ) ;
#1202 = AXIS2_PLACEMENT_3D ( 'NONE', #13414, #4550, #11790 ) ;
#1203 = CYLINDRICAL_SURFACE ( 'NONE', #14853, 2.649999999999992806 ) ;
#1204 = ORIENTED_EDGE ( 'NONE', *, *, #3441, .T. ) ;
#1205 = EDGE_CURVE ( 'NONE', #18729, #276, #10244, .T. ) ;
#1206 = ADVANCED_FACE ( 'NONE', ( #12866 ), #2856, .F. ) ;
#1207 = CARTESIAN_POINT ( 'NONE',  ( 0.000000000000000000, 55.33199130079798778, -10.11537145609316468 ) ) ;
#1208 = DIRECTION ( 'NONE',  ( -0.000000000000000000, -1.000000000000000000, 0.000000000000000000 ) ) ;
#1209 = CARTESIAN_POINT ( 'NONE',  ( 0.000000000000000000, -39.14194549634336084, -40.58063702438384013 ) ) ;
#1210 = ORIENTED_EDGE ( 'NONE', *, *, #9710, .F. ) ;
#1211 = ORIENTED_EDGE ( 'NONE', *, *, #18679, .T. ) ;
#1212 = CARTESIAN_POINT ( 'NONE',  ( 0.000000000000000000, 15.00000000000000000, 0.000000000000000000 ) ) ;
#1213 = ADVANCED_FACE ( 'NONE', ( #14194 ), #4377, .T. ) ;
#1214 = ORIENTED_EDGE ( 'NONE', *, *, #11893, .F. ) ;
#1215 = DIRECTION ( 'NONE',  ( -1.000000000000000000, 0.000000000000000000, -0.000000000000000000 ) ) ;
#1216 = AXIS2_PLACEMENT_3D ( 'NONE', #4208, #12675, #10009 ) ;
#1217 = ADVANCED_FACE ( 'NONE', ( #14378 ), #15990, .F. ) ;
#1218 = DIRECTION ( 'NONE',  ( -1.000000000000000000, 0.000000000000000000, 0.000000000000000000 ) ) ;
#1219 = EDGE_CURVE ( 'NONE', #9771, #12239, #15903, .T. ) ;
#1220 = CARTESIAN_POINT ( 'NONE',  ( -90.00000000009003998, 1.000000000000018208, -5.746271514173173500E-15 ) ) ;
#1221 = ORIENTED_EDGE ( 'NONE', *, *, #283, .T. ) ;
#1222 = CARTESIAN_POINT ( 'NONE',  ( -90.38553543446691663, 1.000000000000018208, -4.784491867360616268 ) ) ;
#1223 = AXIS2_PLACEMENT_3D ( 'NONE', #10505, #17666, #3379 ) ;
#1224 = ORIENTED_EDGE ( 'NONE', *, *, #8262, .F. ) ;
#1226 = CARTESIAN_POINT ( 'NONE',  ( -2.000000000000006661, 3.464101615137750834, 0.000000000000000000 ) ) ;
#1225 = PRODUCT_DEFINITION_CONTEXT ( 'detailed design', #14726, 'design' ) ;
#1227 = DIRECTION ( 'NONE',  ( -1.000000000000000000, -0.000000000000000000, 0.000000000000000000 ) ) ;
#1228 = CYLINDRICAL_SURFACE ( 'NONE', #13927, 28.00000000000000355 ) ;
#1229 = ORIENTED_EDGE ( 'NONE', *, *, #1432, .F. ) ;
#1230 = CARTESIAN_POINT ( 'NONE',  ( 10.00000000000000178, 0.000000000000000000, 0.000000000000000000 ) ) ;
#1232 = ORIENTED_EDGE ( 'NONE', *, *, #1897, .T. ) ;
#1231 = EDGE_CURVE ( 'NONE', #17073, #15243, #5440, .T. ) ;
#1233 = CIRCLE ( 'NONE', #13693, 2.649999999999999467 ) ;
#1234 = ADVANCED_FACE ( 'NONE', ( #6958, #5614 ), #17247, .T. ) ;
#1235 = CARTESIAN_POINT ( 'NONE',  ( 10.00000000000000000, -32.31183295104805353, 46.20417134726119457 ) ) ;
#1236 = CYLINDRICAL_SURFACE ( 'NONE', #689, 2.649999999999999467 ) ;
#1237 = ORIENTED_EDGE ( 'NONE', *, *, #10447, .F. ) ;
#1238 = ORIENTED_EDGE ( 'NONE', *, *, #803, .T. ) ;
#1239 = CARTESIAN_POINT ( 'NONE',  ( 0.2499999999999966416, -8.096141056083448362, 0.000000000000000000 ) ) ;
#1240 = EDGE_CURVE ( 'NONE', #10707, #11571, #11166, .T. ) ;
#1241 = ORIENTED_EDGE ( 'NONE', *, *, #10447, .T. ) ;
#1242 = DIRECTION ( 'NONE',  ( 0.000000000000000000, 0.000000000000000000, 1.000000000000000000 ) ) ;
#1243 = LINE ( 'NONE', #7037, #13136 ) ;
#1244 = EDGE_CURVE ( 'NONE', #16786, #7064, #13313, .T. ) ;
#1245 = AXIS2_PLACEMENT_3D ( 'NONE', #17658, #4603, #10410 ) ;
#1246 = CIRCLE ( 'NONE', #11871, 63.00000000006298961 ) ;
#1247 = ORIENTED_EDGE ( 'NONE', *, *, #111, .T. ) ;
#1248 = ORIENTED_EDGE ( 'NONE', *, *, #16015, .T. ) ;
#1249 = CARTESIAN_POINT ( 'NONE',  ( 2.500000000000000000, -1.768423874527824902, -1.020999999999998353 ) ) ;
#1250 = DIRECTION ( 'NONE',  ( 0.000000000000000000, 0.000000000000000000, 1.000000000000000000 ) ) ;
#1251 = DIRECTION ( 'NONE',  ( -1.000000000000000000, 0.000000000000000000, -0.000000000000000000 ) ) ;
#1252 = DIRECTION ( 'NONE',  ( -0.000000000000000000, 1.000000000000000000, -0.000000000000000000 ) ) ;
#1253 = CARTESIAN_POINT ( 'NONE',  ( 3.061616997868383043E-15, -17.25000000000000355, -25.00000000000000000 ) ) ;
#1254 = CYLINDRICAL_SURFACE ( 'NONE', #12528, 24.00000000002400213 ) ;
#1255 = DIRECTION ( 'NONE',  ( -0.000000000000000000, -0.000000000000000000, 1.000000000000000000 ) ) ;
#1256 = EDGE_LOOP ( 'NONE', ( #7920, #17878, #8134, #16176 ) ) ;
#1257 = DIRECTION ( 'NONE',  ( 0.000000000000000000, 0.000000000000000000, 1.000000000000000000 ) ) ;
#1258 =( REPRESENTATION_RELATIONSHIP ('NONE','NONE', #11014, #8256 ) REPRESENTATION_RELATIONSHIP_WITH_TRANSFORMATION ( #7918 )SHAPE_REPRESENTATION_RELATIONSHIP( ) );
#1259 = AXIS2_PLACEMENT_3D ( 'NONE', #16482, #9231, #15049 ) ;
#1260 = DIRECTION ( 'NONE',  ( -0.000000000000000000, 0.000000000000000000, -1.000000000000000000 ) ) ;
#1261 = DIRECTION ( 'NONE',  ( -0.000000000000000000, -0.000000000000000000, -1.000000000000000000 ) ) ;
#1262 = ORIENTED_EDGE ( 'NONE', *, *, #16911, .T. ) ;
#1263 = ADVANCED_FACE ( 'NONE', ( #18264 ), #18579, .F. ) ;
#1264 = CONTEXT_DEPENDENT_SHAPE_REPRESENTATION ( #9016, #1462 ) ;
#1265 = ORIENTED_EDGE ( 'NONE', *, *, #16333, .T. ) ;
#1266 = ORIENTED_EDGE ( 'NONE', *, *, #17499, .F. ) ;
#1267 = CIRCLE ( 'NONE', #12516, 2.396904916527700102 ) ;
#1268 = FACE_OUTER_BOUND ( 'NONE', #15069, .T. ) ;
#1269 = CARTESIAN_POINT ( 'NONE',  ( 23.48826165280196321, 13.24999999999999467, 0.7426739052322660628 ) ) ;
#1270 = ORIENTED_EDGE ( 'NONE', *, *, #15484, .F. ) ;
#1271 = LINE ( 'NONE', #7065, #7548 ) ;
#1272 = DIRECTION ( 'NONE',  ( -1.000000000000000000, -0.000000000000000000, -0.000000000000000000 ) ) ;
#1273 = EDGE_CURVE ( 'NONE', #15756, #13213, #11787, .T. ) ;
#1274 = DIRECTION ( 'NONE',  ( -1.000000000000000000, -0.000000000000000000, -0.000000000000000000 ) ) ;
#1275 = CARTESIAN_POINT ( 'NONE',  ( 10.00000000000000000, -38.81885513159959800, -40.70683587897998734 ) ) ;
#1276 = LINE ( 'NONE', #5644, #14756 ) ;
#1277 = VERTEX_POINT ( 'NONE', #12642 ) ;
#1278 = DIRECTION ( 'NONE',  ( 1.000000000000000000, -0.000000000000000000, -0.000000000000000000 ) ) ;
#1279 = VERTEX_POINT ( 'NONE', #3788 ) ;
#1280 = EDGE_CURVE ( 'NONE', #3817, #3158, #10552, .T. ) ;
#1281 = CARTESIAN_POINT ( 'NONE',  ( -5.686050877451574337, -5.768780236673276995, -1.000000000000000000 ) ) ;
#1282 = ORIENTED_EDGE ( 'NONE', *, *, #14553, .T. ) ;
#1283 = PRODUCT_CONTEXT ( 'NONE', #13155, 'mechanical' ) ;
#1284 = DIRECTION ( 'NONE',  ( 0.000000000000000000, 0.000000000000000000, -1.000000000000000000 ) ) ;
#1285 = ORIENTED_EDGE ( 'NONE', *, *, #6025, .T. ) ;
#1286 = AXIS2_PLACEMENT_3D ( 'NONE', #17811, #8951, #10577 ) ;
#1287 = ORIENTED_EDGE ( 'NONE', *, *, #12978, .F. ) ;
#1288 = CARTESIAN_POINT ( 'NONE',  ( 0.000000000000000000, 0.5192545390863916310, 0.000000000000000000 ) ) ;
#1289 = LINE ( 'NONE', #14331, #3976 ) ;
#1290 = CYLINDRICAL_SURFACE ( 'NONE', #17578, 33.00000000003299760 ) ;
#1291 = EDGE_CURVE ( 'NONE', #9889, #9794, #9042, .T. ) ;
#1292 = CARTESIAN_POINT ( 'NONE',  ( 10.00000000000000000, 39.14194549634421350, -40.58063702438301590 ) ) ;
#1293 = TOROIDAL_SURFACE ( 'NONE', #11005, 2.700000000000000622, 0.2000000000000000111 ) ;
#1294 = DIRECTION ( 'NONE',  ( 0.000000000000000000, 0.000000000000000000, 1.000000000000000000 ) ) ;
#1295 = VERTEX_POINT ( 'NONE', #2169 ) ;
#1296 = EDGE_CURVE ( 'NONE', #114, #9433, #4484, .T. ) ;
#1297 = DIRECTION ( 'NONE',  ( -1.000000000000000000, -0.000000000000000000, -0.000000000000000000 ) ) ;
#1298 = CARTESIAN_POINT ( 'NONE',  ( -31.74999999999995737, 0.000000000000000000, 4.250000000000000000 ) ) ;
#1299 = CARTESIAN_POINT ( 'NONE',  ( -26.29305231718584324, -26.50000000000000000, 19.10302069950530779 ) ) ;
#1300 = ORIENTED_EDGE ( 'NONE', *, *, #11741, .F. ) ;
#1301 = ORIENTED_EDGE ( 'NONE', *, *, #8671, .T. ) ;
#1302 = LINE ( 'NONE', #13013, #5341 ) ;
#1303 = FILL_AREA_STYLE_COLOUR ( '', #13221 ) ;
#1304 = VERTEX_POINT ( 'NONE', #7975 ) ;
#1305 = EDGE_CURVE ( 'NONE', #2152, #16786, #7212, .T. ) ;
#1306 = AXIS2_PLACEMENT_3D ( 'NONE', #17895, #2175, #10558 ) ;
#1307 = CARTESIAN_POINT ( 'NONE',  ( 2.500000000000000000, -1.178949249685218081, -2.041999999999998039 ) ) ;
#1308 = EDGE_CURVE ( 'NONE', #12068, #9105, #850, .T. ) ;
#1309 = AXIS2_PLACEMENT_3D ( 'NONE', #14116, #10877, #5169 ) ;
#1310 = AXIS2_PLACEMENT_3D ( 'NONE', #293, #10106, #7140 ) ;
#1311 = CARTESIAN_POINT ( 'NONE',  ( -117.1020693116506379, -30.00000000000000000, -19.69080595179801207 ) ) ;
#1312 = ORIENTED_EDGE ( 'NONE', *, *, #2507, .T. ) ;
#1313 = CARTESIAN_POINT ( 'NONE',  ( 0.000000000000000000, 47.29147401532013362, -41.62350880771872852 ) ) ;
#1314 = ORIENTED_EDGE ( 'NONE', *, *, #6426, .T. ) ;
#1315 = CARTESIAN_POINT ( 'NONE',  ( 0.000000000000000000, 1.335003989221626775, 56.23315539212690339 ) ) ;
#1316 = VERTEX_POINT ( 'NONE', #749 ) ;
#1317 = CARTESIAN_POINT ( 'NONE',  ( 10.00000000000000000, -24.33982105418938602, 50.71018745830434682 ) ) ;
#1318 = EDGE_LOOP ( 'NONE', ( #13015, #394, #16969, #60 ) ) ;
#1319 = CARTESIAN_POINT ( 'NONE',  ( -79.64793068852898728, -30.00000000000000000, -29.21039329588757383 ) ) ;
#1320 = DIRECTION ( 'NONE',  ( 0.000000000000000000, 0.000000000000000000, -1.000000000000000000 ) ) ;
#1321 = ORIENTED_EDGE ( 'NONE', *, *, #3129, .T. ) ;
#1322 = ORIENTED_EDGE ( 'NONE', *, *, #10175, .T. ) ;
#1323 = CARTESIAN_POINT ( 'NONE',  ( 5.000000000000000000, 15.68049343256038419, -29.03656532225546627 ) ) ;
#1324 = ORIENTED_EDGE ( 'NONE', *, *, #10853, .T. ) ;
#1325 = DIRECTION ( 'NONE',  ( 1.000000000000000000, 0.000000000000000000, 0.000000000000000000 ) ) ;
#1326 = CARTESIAN_POINT ( 'NONE',  ( 10.00000000000000000, 56.37237871411034007, 1.017308535512583711 ) ) ;
#1327 = CLOSED_SHELL ( 'NONE', ( #17965, #164, #14690, #13540, #3071, #12220, #17855, #6904, #18585, #8315, #17345, #16285, #11966, #5922, #5029, #11411, #5542, #6343, #15976, #1623, #14717, #17295, #12308, #8944, #14474, #5704 ) ) ;
#1328 = EDGE_CURVE ( 'NONE', #10185, #18475, #2082, .T. ) ;
#1329 = DIRECTION ( 'NONE',  ( 0.000000000000000000, 0.000000000000000000, -1.000000000000000000 ) ) ;
#1330 = EDGE_CURVE ( 'NONE', #5282, #4170, #6921, .T. ) ;
#1331 = ADVANCED_FACE ( 'NONE', ( #10924 ), #16748, .F. ) ;
#1332 = VERTEX_POINT ( 'NONE', #13983 ) ;
#1333 = AXIS2_PLACEMENT_3D ( 'NONE', #10419, #8975, #3282 ) ;
#1334 = EDGE_CURVE ( 'NONE', #11781, #17591, #6650, .T. ) ;
#1335 = ORIENTED_EDGE ( 'NONE', *, *, #10484, .T. ) ;
#1336 = DIRECTION ( 'NONE',  ( 0.000000000000000000, 0.000000000000000000, 1.000000000000000000 ) ) ;
#1337 = CARTESIAN_POINT ( 'NONE',  ( -3.861362476283256129, -2.629030857716004199, -3.671615880910374941 ) ) ;
#1338 = DIRECTION ( 'NONE',  ( 0.000000000000000000, -0.3090169943749548342, 0.9510565162951511997 ) ) ;
#1339 = CARTESIAN_POINT ( 'NONE',  ( -90.00000000009003998, 1.000000000000018208, -5.746271514173173500E-15 ) ) ;
#1340 = DIRECTION ( 'NONE',  ( 0.000000000000000000, 0.3090169943749411785, 0.9510565162951556406 ) ) ;
#1341 = CARTESIAN_POINT ( 'NONE',  ( 10.00000000000000000, -55.74967257055887870, 7.478235706488783663 ) ) ;
#1342 = DIRECTION ( 'NONE',  ( 0.000000000000000000, 0.000000000000000000, 1.000000000000000000 ) ) ;
#1343 = EDGE_LOOP ( 'NONE', ( #520, #9190 ) ) ;
#1344 = FACE_OUTER_BOUND ( 'NONE', #5692, .T. ) ;
#1345 = CARTESIAN_POINT ( 'NONE',  ( 10.00000000000000000, -49.49802920186242972, 26.71881558261712186 ) ) ;
#1346 = EDGE_CURVE ( 'NONE', #6013, #15420, #9786, .T. ) ;
#1347 = ORIENTED_EDGE ( 'NONE', *, *, #13438, .F. ) ;
#1348 = CARTESIAN_POINT ( 'NONE',  ( 2.500000000000000000, -1.178949249685214307, 2.042000000000001592 ) ) ;
#1349 = CYLINDRICAL_SURFACE ( 'NONE', #8605, 27.00000000000000355 ) ;
#1350 = COLOUR_RGB ( '',0.8941176470588234615, 0.8941176470588234615, 0.8941176470588234615 ) ;
#1351 = VERTEX_POINT ( 'NONE', #15597 ) ;
#1352 = EDGE_CURVE ( 'NONE', #7394, #3875, #6934, .T. ) ;
#1353 = VERTEX_POINT ( 'NONE', #230 ) ;
#1354 = CARTESIAN_POINT ( 'NONE',  ( 0.000000000000000000, -9.823366686500245137, -55.51919907100663920 ) ) ;
#1355 = CARTESIAN_POINT ( 'NONE',  ( 0.000000000000000000, -24.46385708179976604, -9.514709542737152859 ) ) ;
#1356 = ORIENTED_EDGE ( 'NONE', *, *, #2247, .T. ) ;
#1357 = ADVANCED_FACE ( 'NONE', ( #2542 ), #6031, .T. ) ;
#1358 = LINE ( 'NONE', #15552, #15713 ) ;
#1359 = PRESENTATION_LAYER_ASSIGNMENT (  '', '', ( #438 ) ) ;
#1360 = EDGE_CURVE ( 'NONE', #15153, #18313, #3177, .T. ) ;
#1361 = CARTESIAN_POINT ( 'NONE',  ( 10.00000000000000000, -26.71881558261766898, 49.49802920186213129 ) ) ;
#1362 = DIRECTION ( 'NONE',  ( 1.000000000000000000, 0.000000000000000000, 0.000000000000000000 ) ) ;
#1363 = DIRECTION ( 'NONE',  ( 0.000000000000000000, 0.8090169943749444537, 0.5877852522924772449 ) ) ;
#1364 = ORIENTED_EDGE ( 'NONE', *, *, #3902, .T. ) ;
#1365 = CARTESIAN_POINT ( 'NONE',  ( -4.000000000000000000, 2.309401076758498483, -0.4999999999999927280 ) ) ;
#1366 = VERTEX_POINT ( 'NONE', #10412 ) ;
#1367 = LINE ( 'NONE', #17181, #428 ) ;
#1368 = DIRECTION ( 'NONE',  ( -1.000000000000000000, -0.000000000000000000, 0.000000000000000000 ) ) ;
#1369 = ORIENTED_EDGE ( 'NONE', *, *, #11664, .F. ) ;
#1370 = ORIENTED_EDGE ( 'NONE', *, *, #1440, .F. ) ;
#1371 = VECTOR ( 'NONE', #15439, 1000.000000000000000 ) ;
#1372 = CIRCLE ( 'NONE', #18701, 2.649999999999997691 ) ;
#1373 = CARTESIAN_POINT ( 'NONE',  ( 10.00000000000000000, 40.19788616105610402, 48.50907078259396599 ) ) ;
#1374 = DIRECTION ( 'NONE',  ( 0.000000000000000000, 0.000000000000000000, 1.000000000000000000 ) ) ;
#1375 = LINE ( 'NONE', #13181, #2373 ) ;
#1376 = EDGE_CURVE ( 'NONE', #17330, #6436, #16651, .T. ) ;
#1377 = DIRECTION ( 'NONE',  ( 1.000000000000000000, 0.000000000000000000, 0.000000000000000000 ) ) ;
#1378 = CARTESIAN_POINT ( 'NONE',  ( 0.000000000000000000, 0.000000000000000000, -5.000000000000000000 ) ) ;
#1379 = VERTEX_POINT ( 'NONE', #1129 ) ;
#1380 = DIRECTION ( 'NONE',  ( -1.000000000000000000, -0.000000000000000000, -0.000000000000000000 ) ) ;
#1381 = DIRECTION ( 'NONE',  ( -1.000000000000000000, -0.000000000000000000, -0.000000000000000000 ) ) ;
#1382 = DIRECTION ( 'NONE',  ( -0.000000000000000000, 1.000000000000000000, -0.000000000000000000 ) ) ;
#1383 = ORIENTED_EDGE ( 'NONE', *, *, #3704, .T. ) ;
#1384 = AXIS2_PLACEMENT_3D ( 'NONE', #7473, #17582, #15958 ) ;
#1385 = ORIENTED_EDGE ( 'NONE', *, *, #9563, .T. ) ;
#1386 = AXIS2_PLACEMENT_3D ( 'NONE', #9079, #17661, #4177 ) ;
#1387 = DIRECTION ( 'NONE',  ( -2.031314180040284764E-16, -1.000000000000000000, -1.301042606982601377E-16 ) ) ;
#1388 = ORIENTED_EDGE ( 'NONE', *, *, #13436, .F. ) ;
#1389 = EDGE_CURVE ( 'NONE', #7667, #10934, #11478, .T. ) ;
#1390 = CIRCLE ( 'NONE', #4734, 2.649999999999999467 ) ;
#1391 = EDGE_CURVE ( 'NONE', #7353, #14282, #5087, .T. ) ;
#1392 = CARTESIAN_POINT ( 'NONE',  ( 0.000000000000000000, -1.489278925039700052, 26.20671763660628173 ) ) ;
#1393 = CIRCLE ( 'NONE', #5656, 2.041999999999999815 ) ;
#1395 = AXIS2_PLACEMENT_3D ( 'NONE', #4398, #8866, #7433 ) ;
#1394 = CARTESIAN_POINT ( 'NONE',  ( 10.00000000000000000, 26.20671763660628528, -1.489278925039611901 ) ) ;
#1396 = EDGE_LOOP ( 'NONE', ( #2043, #17843, #11361, #6167 ) ) ;
#1397 = EDGE_LOOP ( 'NONE', ( #11377, #14520, #10547, #14301 ) ) ;
#1398 = FACE_OUTER_BOUND ( 'NONE', #2904, .T. ) ;
#1399 = ORIENTED_EDGE ( 'NONE', *, *, #3782, .T. ) ;
#1400 = CARTESIAN_POINT ( 'NONE',  ( 2.000000000000000444, 3.464101615137754830, -3.142992957459231018 ) ) ;
#1401 = ORIENTED_EDGE ( 'NONE', *, *, #12750, .T. ) ;
#1402 = CYLINDRICAL_SURFACE ( 'NONE', #7880, 7.500000000000007105 ) ;
#1403 = DIRECTION ( 'NONE',  ( 0.000000000000000000, 0.000000000000000000, 1.000000000000000000 ) ) ;
#1404 = AXIS2_PLACEMENT_3D ( 'NONE', #15196, #16895, #9551 ) ;
#1405 = ORIENTED_EDGE ( 'NONE', *, *, #12009, .T. ) ;
#1406 = EDGE_LOOP ( 'NONE', ( #9767, #18125, #1265, #12186 ) ) ;
#1407 = TOROIDAL_SURFACE ( 'NONE', #6865, 5.384454397937118664, 0.5155456020628804703 ) ;
#1408 = FACE_OUTER_BOUND ( 'NONE', #10176, .T. ) ;
#1409 = CIRCLE ( 'NONE', #5665, 63.00000000006298961 ) ;
#1410 = ORIENTED_EDGE ( 'NONE', *, *, #531, .T. ) ;
#1411 = CARTESIAN_POINT ( 'NONE',  ( -4.024497503033714452, -2.323544716729502468, -3.572167766733752803 ) ) ;
#1412 = AXIS2_PLACEMENT_3D ( 'NONE', #15854, #5483, #5761 ) ;
#1413 = VECTOR ( 'NONE', #3052, 1000.000000000000000 ) ;
#1414 = DIRECTION ( 'NONE',  ( 0.000000000000000000, 0.000000000000000000, 1.000000000000000000 ) ) ;
#1415 = AXIS2_PLACEMENT_3D ( 'NONE', #12758, #15515, #11024 ) ;
#1416 = ORIENTED_EDGE ( 'NONE', *, *, #8913, .T. ) ;
#1417 = VECTOR ( 'NONE', #10306, 999.9999999999998863 ) ;
#1418 = CIRCLE ( 'NONE', #12064, 24.00000000002399858 ) ;
#1419 = ORIENTED_EDGE ( 'NONE', *, *, #447, .F. ) ;
#1420 = CARTESIAN_POINT ( 'NONE',  ( 10.00000000000000000, 24.79895094899259789, 13.40641754777674421 ) ) ;
#1421 = AXIS2_PLACEMENT_3D ( 'NONE', #18577, #2952, #17151 ) ;
#1422 = CARTESIAN_POINT ( 'NONE',  ( -4.211140560182196957, 2.431303136016537803, -3.745885042887433514 ) ) ;
#1423 = CYLINDRICAL_SURFACE ( 'NONE', #16347, 40.00000000000000000 ) ;
#1424 = CARTESIAN_POINT ( 'NONE',  ( 0.000000000000000000, 0.000000000000000000, -1.000000000000000000 ) ) ;
#1425 = CARTESIAN_POINT ( 'NONE',  ( -4.204114297095464359, 1.660363174096617156, -3.602136431857887011 ) ) ;
#1426 = DIRECTION ( 'NONE',  ( -1.000000000000000000, 0.000000000000000000, 0.000000000000000000 ) ) ;
#1427 = DIRECTION ( 'NONE',  ( 1.000000000000000000, -0.000000000000000000, 0.000000000000000000 ) ) ;
#1428 = CARTESIAN_POINT ( 'NONE',  ( -90.00000000009001155, -88.00000000000000000, 27.50000000000000000 ) ) ;
#1429 = ORIENTED_EDGE ( 'NONE', *, *, #14244, .F. ) ;
#1430 = DIRECTION ( 'NONE',  ( 0.000000000000000000, 1.000000000000000000, 0.000000000000000000 ) ) ;
#1431 = EDGE_CURVE ( 'NONE', #1351, #1465, #1744, .T. ) ;
#1432 = EDGE_CURVE ( 'NONE', #9337, #5360, #326, .T. ) ;
#1433 = CARTESIAN_POINT ( 'NONE',  ( 0.000000000000000000, 11.24999999999999645, 0.000000000000000000 ) ) ;
#1434 = ADVANCED_FACE ( 'NONE', ( #13274 ), #17042, .T. ) ;
#1435 = VERTEX_POINT ( 'NONE', #14273 ) ;
#1436 = DIRECTION ( 'NONE',  ( 1.000000000000000000, -2.031314180040284764E-16, 0.000000000000000000 ) ) ;
#1437 = FACE_BOUND ( 'NONE', #12860, .T. ) ;
#1438 = AXIS2_PLACEMENT_3D ( 'NONE', #10845, #12667, #875 ) ;
#1439 = AXIS2_PLACEMENT_3D ( 'NONE', #1230, #16844, #18268 ) ;
#1440 = EDGE_CURVE ( 'NONE', #1277, #9572, #17130, .T. ) ;
#1441 = ORIENTED_EDGE ( 'NONE', *, *, #14547, .F. ) ;
#1442 = AXIS2_PLACEMENT_3D ( 'NONE', #14267, #11299, #17126 ) ;
#1443 = AXIS2_PLACEMENT_3D ( 'NONE', #14790, #8968, #7556 ) ;
#1444 = ORIENTED_EDGE ( 'NONE', *, *, #17033, .F. ) ;
#1445 = DIRECTION ( 'NONE',  ( 0.000000000000000000, 0.000000000000000000, 1.000000000000000000 ) ) ;
#1446 = DIRECTION ( 'NONE',  ( -0.5000000000000051070, 0.000000000000000000, 0.8660254037844355990 ) ) ;
#1447 = ADVANCED_FACE ( 'NONE', ( #16139 ), #17217, .F. ) ;
#1448 = VECTOR ( 'NONE', #16372, 1000.000000000000000 ) ;
#1449 = EDGE_LOOP ( 'NONE', ( #12624, #5261 ) ) ;
#1450 = CARTESIAN_POINT ( 'NONE',  ( 0.000000000000000000, -9.514709542737069370, 24.46385708179980512 ) ) ;
#1451 = DIRECTION ( 'NONE',  ( 0.000000000000000000, 0.000000000000000000, -1.000000000000000000 ) ) ;
#1452 = CIRCLE ( 'NONE', #12089, 2.649999999999999467 ) ;
#1453 = DIRECTION ( 'NONE',  ( -0.000000000000000000, 1.000000000000000000, -0.000000000000000000 ) ) ;
#1454 = DIRECTION ( 'NONE',  ( -0.000000000000000000, -0.000000000000000000, 1.000000000000000000 ) ) ;
#1455 = CARTESIAN_POINT ( 'NONE',  ( 10.00000000000000000, 0.000000000000000000, 0.000000000000000000 ) ) ;
#1456 = ORIENTED_EDGE ( 'NONE', *, *, #14822, .T. ) ;
#1457 = AXIS2_PLACEMENT_3D ( 'NONE', #120, #5912, #4495 ) ;
#1458 = DIRECTION ( 'NONE',  ( -0.000000000000000000, -1.000000000000000000, -0.000000000000000000 ) ) ;
#1459 = ORIENTED_EDGE ( 'NONE', *, *, #15588, .F. ) ;
#1460 = EDGE_CURVE ( 'NONE', #9528, #7635, #226, .T. ) ;
#1461 = EDGE_CURVE ( 'NONE', #4891, #11483, #65, .T. ) ;
#1462 = PRODUCT_DEFINITION_SHAPE ( 'NONE', 'NONE',  #18846 ) ;
#1463 = DIRECTION ( 'NONE',  ( 0.000000000000000000, -0.5877852522924801315, 0.8090169943749421222 ) ) ;
#1464 = DIRECTION ( 'NONE',  ( 0.000000000000000000, 0.000000000000000000, 1.000000000000000000 ) ) ;
#1465 = VERTEX_POINT ( 'NONE', #14612 ) ;
#1466 = SHAPE_DEFINITION_REPRESENTATION ( #10584, #16742 ) ;
#1467 = ORIENTED_EDGE ( 'NONE', *, *, #1019, .T. ) ;
#1468 = AXIS2_PLACEMENT_3D ( 'NONE', #18555, #9500, #6546 ) ;
#1469 = EDGE_CURVE ( 'NONE', #14358, #11663, #5702, .T. ) ;
#1470 = VECTOR ( 'NONE', #589, 1000.000000000000000 ) ;
#1471 = AXIS2_PLACEMENT_3D ( 'NONE', #4788, #17833, #10597 ) ;
#1472 = VECTOR ( 'NONE', #774, 1000.000000000000000 ) ;
#1473 = DIRECTION ( 'NONE',  ( 1.000000000000000000, 0.000000000000000000, 0.000000000000000000 ) ) ;
#1474 = CARTESIAN_POINT ( 'NONE',  ( 3.309651814758565180, -5.455921364805393026, -1.000000000000000000 ) ) ;
#1475 = DIRECTION ( 'NONE',  ( -1.000000000000000000, -0.000000000000000000, -0.000000000000000000 ) ) ;
#1476 = FACE_OUTER_BOUND ( 'NONE', #11507, .T. ) ;
#1477 = CIRCLE ( 'NONE', #13629, 63.00000000006298961 ) ;
#1478 = CARTESIAN_POINT ( 'NONE',  ( 0.000000000000000000, -23.24033432160480217, 58.55669782892453412 ) ) ;
#1479 = ORIENTED_EDGE ( 'NONE', *, *, #10684, .F. ) ;
#1480 = AXIS2_PLACEMENT_3D ( 'NONE', #15914, #11251, #1062 ) ;
#1481 = DIRECTION ( 'NONE',  ( 0.000000000000000000, 0.5877852522924741363, -0.8090169943749465631 ) ) ;
#1482 = CARTESIAN_POINT ( 'NONE',  ( 10.00000000000000000, -38.81885513160016643, 40.70683587897944022 ) ) ;
#1483 = DIRECTION ( 'NONE',  ( 0.000000000000000000, 0.000000000000000000, 1.000000000000000000 ) ) ;
#1484 = CIRCLE ( 'NONE', #6347, 24.00000000002400213 ) ;
#1485 = ORIENTED_EDGE ( 'NONE', *, *, #7965, .F. ) ;
#1486 = VERTEX_POINT ( 'NONE', #13184 ) ;
#1487 = CIRCLE ( 'NONE', #6349, 23.50000000000000355 ) ;
#1488 = CARTESIAN_POINT ( 'NONE',  ( 0.000000000000000000, -56.37237871411034718, 25.01730853553617351 ) ) ;
#1489 = VERTEX_POINT ( 'NONE', #4516 ) ;
#1490 = EDGE_CURVE ( 'NONE', #6043, #18269, #12019, .T. ) ;
#1491 = VECTOR ( 'NONE', #18744, 1000.000000000000000 ) ;
#1492 = CARTESIAN_POINT ( 'NONE',  ( -26.29305231718568336, -30.00000000000000000, -21.75302069950551953 ) ) ;
#1493 = CYLINDRICAL_SURFACE ( 'NONE', #7446, 56.24900000005625600 ) ;
#1494 = VECTOR ( 'NONE', #7308, 1000.000000000000000 ) ;
#1495 = DIRECTION ( 'NONE',  ( 0.8660254037844374864, -0.5000000000000018874, 0.000000000000000000 ) ) ;
#1496 = VERTEX_POINT ( 'NONE', #13828 ) ;
#1497 = DIRECTION ( 'NONE',  ( 0.000000000000000000, 1.000000000000000000, 3.469446951950143595E-15 ) ) ;
#1498 = ORIENTED_EDGE ( 'NONE', *, *, #3408, .T. ) ;
#1499 = CARTESIAN_POINT ( 'NONE',  ( 10.00000000000000000, 62.72529079327805590, 5.876895005582662534 ) ) ;
#1500 = ORIENTED_EDGE ( 'NONE', *, *, #14129, .F. ) ;
#1501 = VERTEX_POINT ( 'NONE', #10599 ) ;
#1502 = ADVANCED_FACE ( 'NONE', ( #10876 ), #16316, .F. ) ;
#1503 = CARTESIAN_POINT ( 'NONE',  ( 4.000000000000000000, -2.309401076758514915, -3.433295621305383349 ) ) ;
#1504 = LINE ( 'NONE', #4443, #15007 ) ;
#1505 = AXIS2_PLACEMENT_3D ( 'NONE', #11559, #6881, #12702 ) ;
#1506 = ORIENTED_EDGE ( 'NONE', *, *, #17282, .F. ) ;
#1507 = VERTEX_POINT ( 'NONE', #9356 ) ;
#1508 = CARTESIAN_POINT ( 'NONE',  ( 0.000000000000000000, 0.000000000000000000, -4.974599999999998801 ) ) ;
#1509 = CIRCLE ( 'NONE', #14580, 2.041999999999999815 ) ;
#1510 = ADVANCED_FACE ( 'NONE', ( #15262, #2212 ), #17837, .T. ) ;
#1511 =( NAMED_UNIT ( * ) PLANE_ANGLE_UNIT ( ) SI_UNIT ( $, .RADIAN. ) );
#1512 = ORIENTED_EDGE ( 'NONE', *, *, #4100, .T. ) ;
#1513 = DIRECTION ( 'NONE',  ( -0.000000000000000000, 1.000000000000000000, -0.000000000000000000 ) ) ;
#1514 = DIRECTION ( 'NONE',  ( 0.000000000000000000, 0.000000000000000000, 1.000000000000000000 ) ) ;
#1515 = AXIS2_PLACEMENT_3D ( 'NONE', #7052, #14200, #1257 ) ;
#1516 = EDGE_LOOP ( 'NONE', ( #10443, #4352 ) ) ;
#1517 = ORIENTED_EDGE ( 'NONE', *, *, #17830, .T. ) ;
#1518 = CARTESIAN_POINT ( 'NONE',  ( 10.00000000000000000, -24.68609584167194981, 50.69000562871634230 ) ) ;
#1519 = FACE_OUTER_BOUND ( 'NONE', #1696, .T. ) ;
#1520 = CARTESIAN_POINT ( 'NONE',  ( 10.04305231718579705, -26.50000000000000000, 30.90933677959249337 ) ) ;
#1521 = EDGE_LOOP ( 'NONE', ( #1285, #15685, #17663, #2177 ) ) ;
#1522 = CARTESIAN_POINT ( 'NONE',  ( 0.000000000000000000, 0.000000000000000000, 0.000000000000000000 ) ) ;
#1523 = DIRECTION ( 'NONE',  ( -1.000000000000000000, 0.000000000000000000, 0.000000000000000000 ) ) ;
#1524 = LINE ( 'NONE', #13055, #14054 ) ;
#1525 = DIRECTION ( 'NONE',  ( 0.000000000000000000, -0.000000000000000000, 1.000000000000000000 ) ) ;
#1526 = ORIENTED_EDGE ( 'NONE', *, *, #15585, .F. ) ;
#1527 = CARTESIAN_POINT ( 'NONE',  ( -90.00000000009001155, 2.000000000000001776, -1.301042606982603940E-15 ) ) ;
#1528 = CYLINDRICAL_SURFACE ( 'NONE', #2024, 5.000000000000000000 ) ;
#1529 = EDGE_LOOP ( 'NONE', ( #15960, #3595, #8090, #14721 ) ) ;
#1530 = DIRECTION ( 'NONE',  ( 1.000000000000000000, 0.000000000000000000, 0.000000000000000000 ) ) ;
#1531 = VECTOR ( 'NONE', #8156, 1000.000000000000000 ) ;
#1532 = DIRECTION ( 'NONE',  ( 0.000000000000000000, -1.000000000000000000, 0.000000000000000000 ) ) ;
#1533 = CIRCLE ( 'NONE', #16133, 27.00000000000000355 ) ;
#1534 = VECTOR ( 'NONE', #18328, 1000.000000000000000 ) ;
#1535 = ADVANCED_FACE ( 'NONE', ( #3275 ), #6125, .T. ) ;
#1536 = VERTEX_POINT ( 'NONE', #8018 ) ;
#1537 = FACE_OUTER_BOUND ( 'NONE', #18276, .T. ) ;
#1538 = EDGE_CURVE ( 'NONE', #2152, #15880, #13469, .T. ) ;
#1539 = DIRECTION ( 'NONE',  ( -1.000000000000000000, -0.000000000000000000, -0.000000000000000000 ) ) ;
#1540 = ORIENTED_EDGE ( 'NONE', *, *, #641, .F. ) ;
#1541 = FACE_OUTER_BOUND ( 'NONE', #10983, .T. ) ;
#1542 = AXIS2_PLACEMENT_3D ( 'NONE', #15260, #10682, #12403 ) ;
#1543 = PRODUCT_DEFINITION ( 'UNKNOWN', '', #10800, #17216 ) ;
#1544 = DIRECTION ( 'NONE',  ( -1.000000000000000000, -0.000000000000000000, 0.000000000000000000 ) ) ;
#1545 = CARTESIAN_POINT ( 'NONE',  ( 10.00000000000000000, 40.70683587897958944, 38.81885513160003143 ) ) ;
#1546 = CARTESIAN_POINT ( 'NONE',  ( 10.00000000000000000, 56.23315539212690339, 1.335003989221828835 ) ) ;
#1547 = ORIENTED_EDGE ( 'NONE', *, *, #11386, .T. ) ;
#1548 = CARTESIAN_POINT ( 'NONE',  ( 10.00000000000000000, -6.681932690256794594, -25.38428207620328791 ) ) ;
#1549 = ORIENTED_EDGE ( 'NONE', *, *, #3017, .T. ) ;
#1550 = CARTESIAN_POINT ( 'NONE',  ( 10.00000000000000000, -22.07705612348828694, -14.19907017806892569 ) ) ;
#1551 = DIRECTION ( 'NONE',  ( 0.000000000000000000, -1.000000000000000000, 0.000000000000000000 ) ) ;
#1552 = ORIENTED_EDGE ( 'NONE', *, *, #8041, .T. ) ;
#1553 = APPLICATION_PROTOCOL_DEFINITION ( 'draft international standard', 'automotive_design', 1998, #4630 ) ;
#1554 = ORIENTED_EDGE ( 'NONE', *, *, #12394, .F. ) ;
#1555 = EDGE_CURVE ( 'NONE', #16736, #17488, #9076, .T. ) ;
#1556 = CIRCLE ( 'NONE', #2153, 56.24900000005625600 ) ;
#1557 = EDGE_CURVE ( 'NONE', #7366, #1171, #10497, .T. ) ;
#1558 = FACE_OUTER_BOUND ( 'NONE', #2676, .T. ) ;
#1559 = EDGE_CURVE ( 'NONE', #15687, #2365, #4194, .T. ) ;
#1560 = CYLINDRICAL_SURFACE ( 'NONE', #11255, 12.00000000001200462 ) ;
#1561 = CARTESIAN_POINT ( 'NONE',  ( 0.000000000000000000, 38.81885513159988932, 40.70683587897971734 ) ) ;
#1562 = CARTESIAN_POINT ( 'NONE',  ( -2.500000000000000444, 3.061616997868383634E-16, -5.000000000000000888 ) ) ;
#1563 = ADVANCED_FACE ( 'NONE', ( #7644 ), #6216, .T. ) ;
#1564 = CARTESIAN_POINT ( 'NONE',  ( 10.00000000000000000, 40.58063702438398224, -39.14194549634321163 ) ) ;
#1565 = DIRECTION ( 'NONE',  ( 0.000000000000000000, 0.000000000000000000, 1.000000000000000000 ) ) ;
#1566 = LINE ( 'NONE', #416, #3002 ) ;
#1567 = VERTEX_POINT ( 'NONE', #16419 ) ;
#1568 = EDGE_CURVE ( 'NONE', #11050, #10381, #18115, .T. ) ;
#1569 = AXIS2_PLACEMENT_3D ( 'NONE', #16065, #4538, #4625 ) ;
#1570 = FACE_OUTER_BOUND ( 'NONE', #1521, .T. ) ;
#1571 = CARTESIAN_POINT ( 'NONE',  ( -10.00000000000000000, 0.000000000000000000, 0.000000000000000000 ) ) ;
#1572 = CYLINDRICAL_SURFACE ( 'NONE', #10340, 12.00000000001200817 ) ;
#1573 = ORIENTED_EDGE ( 'NONE', *, *, #8580, .T. ) ;
#1574 = ORIENTED_EDGE ( 'NONE', *, *, #6302, .T. ) ;
#1575 = FACE_BOUND ( 'NONE', #4154, .T. ) ;
#1576 = EDGE_CURVE ( 'NONE', #16034, #9749, #10261, .T. ) ;
#1577 = VECTOR ( 'NONE', #7534, 1000.000000000000000 ) ;
#1578 = EDGE_LOOP ( 'NONE', ( #10752, #1617, #6248, #8159 ) ) ;
#1579 = DIRECTION ( 'NONE',  ( -1.000000000000000000, 0.000000000000000000, 0.000000000000000000 ) ) ;
#1580 = DIRECTION ( 'NONE',  ( 0.000000000000000000, 0.000000000000000000, 1.000000000000000000 ) ) ;
#1581 = FACE_OUTER_BOUND ( 'NONE', #16566, .T. ) ;
#1582 = ORIENTED_EDGE ( 'NONE', *, *, #15882, .F. ) ;
#1583 = CARTESIAN_POINT ( 'NONE',  ( -26.29305231718568336, -26.50000000000000000, -16.45302069950552237 ) ) ;
#1584 = AXIS2_PLACEMENT_3D ( 'NONE', #11711, #17616, #5719 ) ;
#1585 = ORIENTED_EDGE ( 'NONE', *, *, #17375, .F. ) ;
#1586 = DIRECTION ( 'NONE',  ( 0.000000000000000000, 0.000000000000000000, -1.000000000000000000 ) ) ;
#1587 = ORIENTED_EDGE ( 'NONE', *, *, #7596, .F. ) ;
#1588 = ADVANCED_FACE ( 'NONE', ( #3656 ), #14986, .T. ) ;
#1589 = ORIENTED_EDGE ( 'NONE', *, *, #12739, .T. ) ;
#1590 = CARTESIAN_POINT ( 'NONE',  ( -90.00000000009001155, 2.000000000000001776, -5.000000000000005329 ) ) ;
#1591 = DIRECTION ( 'NONE',  ( -0.000000000000000000, 1.000000000000000000, -0.000000000000000000 ) ) ;
#1592 = EDGE_LOOP ( 'NONE', ( #11082, #13432 ) ) ;
#1593 = ORIENTED_EDGE ( 'NONE', *, *, #16015, .F. ) ;
#1594 = FACE_OUTER_BOUND ( 'NONE', #1870, .T. ) ;
#1595 =( NAMED_UNIT ( * ) SI_UNIT ( $, .STERADIAN. ) SOLID_ANGLE_UNIT ( ) );
#1596 = CIRCLE ( 'NONE', #8884, 24.00000000002400213 ) ;
#1597 = ORIENTED_EDGE ( 'NONE', *, *, #705, .F. ) ;
#1598 = FACE_OUTER_BOUND ( 'NONE', #11351, .T. ) ;
#1599 = AXIS2_PLACEMENT_3D ( 'NONE', #9692, #1130, #14274 ) ;
#1600 = CARTESIAN_POINT ( 'NONE',  ( 0.000000000000000000, 55.83748330407408389, -7.813799127873475747 ) ) ;
#1601 = ORIENTED_EDGE ( 'NONE', *, *, #16635, .F. ) ;
#1602 = PRODUCT_DEFINITION_SHAPE ( 'NONE', 'NONE',  #18835 ) ;
#1603 = ORIENTED_EDGE ( 'NONE', *, *, #2146, .F. ) ;
#1604 = FACE_BOUND ( 'NONE', #5895, .T. ) ;
#1605 = CARTESIAN_POINT ( 'NONE',  ( -31.74999999999995737, 3.061616997868383634E-16, -2.500000000000000444 ) ) ;
#1606 = CARTESIAN_POINT ( 'NONE',  ( 0.000000000000000000, 1.017308535512385870, 56.37237871411034007 ) ) ;
#1607 = ORIENTED_EDGE ( 'NONE', *, *, #13546, .F. ) ;
#1608 = DIRECTION ( 'NONE',  ( 0.000000000000000000, -0.5877852522924623679, -0.8090169943749552228 ) ) ;
#1609 = EDGE_CURVE ( 'NONE', #15264, #2861, #7927, .T. ) ;
#1610 = AXIS2_PLACEMENT_3D ( 'NONE', #7959, #732, #14925 ) ;
#1611 = DIRECTION ( 'NONE',  ( -1.000000000000000000, -0.000000000000000000, -0.000000000000000000 ) ) ;
#1612 = CARTESIAN_POINT ( 'NONE',  ( 10.00000000000000000, 7.813799127874054840, -55.83748330407399152 ) ) ;
#1613 = DIRECTION ( 'NONE',  ( -1.000000000000000000, 0.000000000000000000, 0.000000000000000000 ) ) ;
#1614 = ORIENTED_EDGE ( 'NONE', *, *, #7145, .F. ) ;
#1615 = DIRECTION ( 'NONE',  ( 1.000000000000000000, 0.000000000000000000, 0.000000000000000000 ) ) ;
#1616 = DIRECTION ( 'NONE',  ( 0.000000000000000000, 0.000000000000000000, 1.000000000000000000 ) ) ;
#1617 = ORIENTED_EDGE ( 'NONE', *, *, #14824, .T. ) ;
#1618 = DIRECTION ( 'NONE',  ( 1.000000000000000000, -0.000000000000000000, -0.000000000000000000 ) ) ;
#1619 = FACE_OUTER_BOUND ( 'NONE', #15171, .T. ) ;
#1620 = EDGE_CURVE ( 'NONE', #3988, #12362, #508, .T. ) ;
#1621 = AXIS2_PLACEMENT_3D ( 'NONE', #12912, #18712, #5672 ) ;
#1622 = ORIENTED_EDGE ( 'NONE', *, *, #447, .T. ) ;
#1623 = ADVANCED_FACE ( 'NONE', ( #6315, #6500 ), #17936, .F. ) ;
#1624 = LINE ( 'NONE', #17534, #2968 ) ;
#1625 = LINE ( 'NONE', #11725, #320 ) ;
#1626 = VERTEX_POINT ( 'NONE', #18597 ) ;
#1627 = CARTESIAN_POINT ( 'NONE',  ( 10.00000000000000000, 32.46095361140692859, 5.940243314904329885 ) ) ;
#1628 = CARTESIAN_POINT ( 'NONE',  ( 10.00000000000000000, 0.000000000000000000, 0.000000000000000000 ) ) ;
#1629 = CARTESIAN_POINT ( 'NONE',  ( -31.74999999999995737, 0.000000000000000000, 4.250000000000000000 ) ) ;
#1630 = DIRECTION ( 'NONE',  ( 0.000000000000000000, -0.8090169943749401238, -0.5877852522924831291 ) ) ;
#1631 = ORIENTED_EDGE ( 'NONE', *, *, #10360, .T. ) ;
#1632 = CARTESIAN_POINT ( 'NONE',  ( 0.000000000000000000, 22.07705612348859958, -14.19907017806844252 ) ) ;
#1633 = EDGE_LOOP ( 'NONE', ( #4393, #14259, #6883, #4525 ) ) ;
#1634 = AXIS2_PLACEMENT_3D ( 'NONE', #18799, #15751, #1463 ) ;
#1635 = CARTESIAN_POINT ( 'NONE',  ( 0.000000000000000000, 0.000000000000000000, 30.00000000000000000 ) ) ;
#1636 = ORIENTED_EDGE ( 'NONE', *, *, #1042, .T. ) ;
#1637 = SHAPE_DEFINITION_REPRESENTATION ( #11496, #11014 ) ;
#1638 = ORIENTED_EDGE ( 'NONE', *, *, #5200, .T. ) ;
#1639 = MECHANICAL_DESIGN_GEOMETRIC_PRESENTATION_REPRESENTATION (  '', ( #5608 ), #8941 ) ;
#1640 = CYLINDRICAL_SURFACE ( 'NONE', #9296, 5.000000000000000000 ) ;
#1641 = DIRECTION ( 'NONE',  ( 0.000000000000000000, 0.8660254037844380415, -0.5000000000000012212 ) ) ;
#1642 = CARTESIAN_POINT ( 'NONE',  ( -0.2500000000000000000, -8.096141056083446585, 0.000000000000000000 ) ) ;
#1643 = B_SPLINE_CURVE_WITH_KNOTS ( 'NONE', 3,
 ( #4932, #9027, #7780, #1798 ),
 .UNSPECIFIED., .F., .F.,
 ( 4, 4 ),
 ( 0.000000000000000000, 0.002452478801916376308 ),
 .UNSPECIFIED. ) ;
#1644 = CARTESIAN_POINT ( 'NONE',  ( 10.00000000000000000, 0.000000000000000000, 0.000000000000000000 ) ) ;
#1645 = CARTESIAN_POINT ( 'NONE',  ( -87.43997332177200121, -10.00000000000001954, 6.475821446449875118 ) ) ;
#1646 = DIRECTION ( 'NONE',  ( 0.000000000000000000, 1.000000000000000000, 0.000000000000000000 ) ) ;
#1647 = CARTESIAN_POINT ( 'NONE',  ( -290.0000000000001137, -34.99999999999999289, -125.0000000000000000 ) ) ;
#1648 = ORIENTED_EDGE ( 'NONE', *, *, #5400, .T. ) ;
#1649 =( BOUNDED_SURFACE ( )  B_SPLINE_SURFACE ( 3, 2, ( 
 ( #10852, #3639, #8002 ),
 ( #12486, #18291, #13813 ),
 ( #12388, #14387, #14470 ),
 ( #17074, #17350, #9816 ),
 ( #18672, #16970, #15628 ),
 ( #11142, #9906, #12958 ) ),
 .UNSPECIFIED., .F., .F., .F. ) 
 B_SPLINE_SURFACE_WITH_KNOTS ( ( 4, 2, 4 ),
 ( 3, 3 ),
 ( 0.02032853247518126918, 0.02278863295364821906, 0.02524873343211516893 ),
 ( 0.000000000000000000, 1.000000000000000000 ),
 .UNSPECIFIED. ) 
 GEOMETRIC_REPRESENTATION_ITEM ( )  RATIONAL_B_SPLINE_SURFACE ( (
 ( 1.000000000000000000, 0.8047781615896838492, 1.000000000000000000),
 ( 1.000000000000000000, 0.8123767586288186404, 1.000000000000000000),
 ( 1.000000000000000000, 0.8190662415565814758, 1.000000000000000000),
 ( 1.000000000000000000, 0.8192361015667604107, 1.000000000000000000),
 ( 1.000000000000000000, 0.8126135807104967190, 1.000000000000000000),
 ( 1.000000000000000000, 0.8047712338318580017, 1.000000000000000000) ) ) 
 REPRESENTATION_ITEM ( '' )  SURFACE ( )  );
#1650 = SURFACE_SIDE_STYLE ('',( #14703 ) ) ;
#1651 = CARTESIAN_POINT ( 'NONE',  ( 10.00000000000000000, 9.514709542737238124, -24.46385708179973406 ) ) ;
#1652 = FACE_OUTER_BOUND ( 'NONE', #6703, .T. ) ;
#1653 = VERTEX_POINT ( 'NONE', #8502 ) ;
#1654 = EDGE_LOOP ( 'NONE', ( #3997, #6945 ) ) ;
#1655 = ADVANCED_FACE ( 'NONE', ( #1077 ), #6982, .T. ) ;
#1656 = EDGE_CURVE ( 'NONE', #2709, #2599, #1182, .T. ) ;
#1657 = CARTESIAN_POINT ( 'NONE',  ( 10.00000000000000000, 55.83748330407408389, 16.18620087215052195 ) ) ;
#1658 = CARTESIAN_POINT ( 'NONE',  ( 0.000000000000000000, 0.000000000000000000, 0.000000000000000000 ) ) ;
#1659 = PRESENTATION_LAYER_ASSIGNMENT (  '', '', ( #3801 ) ) ;
#1661 = EDGE_CURVE ( 'NONE', #16801, #16490, #12405, .T. ) ;
#1660 = CARTESIAN_POINT ( 'NONE',  ( 10.00000000000000000, 0.000000000000000000, 0.000000000000000000 ) ) ;
#1662 = ORIENTED_EDGE ( 'NONE', *, *, #10152, .T. ) ;
#1663 = CIRCLE ( 'NONE', #12299, 12.00000000001200284 ) ;
#1664 = EDGE_CURVE ( 'NONE', #15420, #16109, #13016, .T. ) ;
#1665 = EDGE_CURVE ( 'NONE', #1489, #15209, #9351, .T. ) ;
#1666 = DIRECTION ( 'NONE',  ( 0.1416665029469836024, 0.000000000000000000, 0.9899144417285627995 ) ) ;
#1667 = CARTESIAN_POINT ( 'NONE',  ( 1.257172072275274388, -3.892973519170983110, -3.433252694550781303 ) ) ;
#1668 = CARTESIAN_POINT ( 'NONE',  ( 2.500000000000000000, 1.178949249685212974, -2.042000000000001148 ) ) ;
#1669 = ORIENTED_EDGE ( 'NONE', *, *, #6473, .F. ) ;
#1670 = DIRECTION ( 'NONE',  ( -0.000000000000000000, 0.000000000000000000, 1.000000000000000000 ) ) ;
#1671 = CIRCLE ( 'NONE', #10918, 2.500000000000000444 ) ;
#1672 = AXIS2_PLACEMENT_3D ( 'NONE', #3878, #2251, #11206 ) ;
#1673 = ORIENTED_EDGE ( 'NONE', *, *, #14938, .F. ) ;
#1674 = CARTESIAN_POINT ( 'NONE',  ( 0.000000000000000000, 40.70683587898012235, -38.81885513159945589 ) ) ;
#1675 = AXIS2_PLACEMENT_3D ( 'NONE', #9927, #15556, #991 ) ;
#1676 = ORIENTED_EDGE ( 'NONE', *, *, #10639, .F. ) ;
#1677 = DIRECTION ( 'NONE',  ( -2.031314180040284764E-16, -1.000000000000000000, -1.301042606982601377E-16 ) ) ;
#1678 = CYLINDRICAL_SURFACE ( 'NONE', #5863, 56.24900000005625600 ) ;
#1679 = ORIENTED_EDGE ( 'NONE', *, *, #9992, .T. ) ;
#1680 = EDGE_LOOP ( 'NONE', ( #2596, #9124, #12279, #78 ) ) ;
#1681 = EDGE_CURVE ( 'NONE', #3221, #14211, #7538, .T. ) ;
#1682 = CARTESIAN_POINT ( 'NONE',  ( 0.000000000000000000, -20.32630374611196800, 16.60877409751161693 ) ) ;
#1683 = VERTEX_POINT ( 'NONE', #16885 ) ;
#1684 = CARTESIAN_POINT ( 'NONE',  ( 10.00000000000000000, 0.000000000000000000, 0.000000000000000000 ) ) ;
#1685 = CIRCLE ( 'NONE', #18724, 4.799999999999999822 ) ;
#1686 = AXIS2_PLACEMENT_3D ( 'NONE', #5238, #13727, #9149 ) ;
#1687 = EDGE_CURVE ( 'NONE', #7353, #5299, #3597, .T. ) ;
#1688 = DIRECTION ( 'NONE',  ( 0.000000000000000000, 0.3090169943749480619, -0.9510565162951533091 ) ) ;
#1689 = EDGE_LOOP ( 'NONE', ( #1498, #18620, #13343, #3428 ) ) ;
#1690 = CIRCLE ( 'NONE', #2305, 63.00000000006298961 ) ;
#1691 = VERTEX_POINT ( 'NONE', #6788 ) ;
#1692 = DIRECTION ( 'NONE',  ( 0.000000000000000000, 0.000000000000000000, -1.000000000000000000 ) ) ;
#1693 = DIRECTION ( 'NONE',  ( 0.000000000000000000, 1.000000000000000000, 0.000000000000000000 ) ) ;
#1695 = AXIS2_PLACEMENT_3D ( 'NONE', #1846, #13475, #418 ) ;
#1694 = FACE_OUTER_BOUND ( 'NONE', #14322, .T. ) ;
#1696 = EDGE_LOOP ( 'NONE', ( #10398, #5674, #5841, #2401 ) ) ;
#1697 = CARTESIAN_POINT ( 'NONE',  ( -4.000000000000000000, 0.8730739991738342143, -3.223134629628428893 ) ) ;
#1698 = CARTESIAN_POINT ( 'NONE',  ( 0.000000000000000000, 0.000000000000000000, 0.000000000000000000 ) ) ;
#1699 = DIRECTION ( 'NONE',  ( -1.000000000000000000, -0.000000000000000000, 0.000000000000000000 ) ) ;
#1700 = DIRECTION ( 'NONE',  ( 0.000000000000000000, 1.000000000000000000, 0.000000000000000000 ) ) ;
#1701 = ORIENTED_EDGE ( 'NONE', *, *, #15947, .F. ) ;
#1702 = CARTESIAN_POINT ( 'NONE',  ( 10.00000000000000000, -49.76630880786327538, 26.49895292617986797 ) ) ;
#1703 = VECTOR ( 'NONE', #11338, 1000.000000000000000 ) ;
#1704 = LINE ( 'NONE', #664, #14185 ) ;
#1705 = ORIENTED_EDGE ( 'NONE', *, *, #18797, .T. ) ;
#1706 = LINE ( 'NONE', #10461, #2400 ) ;
#1707 = FACE_BOUND ( 'NONE', #9784, .T. ) ;
#1708 = APPLICATION_CONTEXT ( 'automotive_design' ) ;
#1709 = AXIS2_PLACEMENT_3D ( 'NONE', #3286, #16430, #8983 ) ;
#1710 = ADVANCED_FACE ( 'NONE', ( #9924 ), #17174, .F. ) ;
#1711 = CIRCLE ( 'NONE', #14792, 63.00000000006298961 ) ;
#1712 = VECTOR ( 'NONE', #637, 1000.000000000000000 ) ;
#1713 = ORIENTED_EDGE ( 'NONE', *, *, #5547, .T. ) ;
#1714 = DIRECTION ( 'NONE',  ( -1.000000000000000000, 0.000000000000000000, 0.000000000000000000 ) ) ;
#1715 = DIRECTION ( 'NONE',  ( -1.000000000000000000, 0.000000000000000000, 0.000000000000000000 ) ) ;
#1716 = EDGE_LOOP ( 'NONE', ( #10886, #17650, #17205, #12206 ) ) ;
#1717 = DIRECTION ( 'NONE',  ( -1.000000000000000000, -0.000000000000000000, -0.000000000000000000 ) ) ;
#1718 = CARTESIAN_POINT ( 'NONE',  ( 2.500000000000000000, 1.178949249685213863, -2.042000000000001148 ) ) ;
#1719 = DIRECTION ( 'NONE',  ( -1.000000000000000000, -0.000000000000000000, -0.000000000000000000 ) ) ;
#1720 = CARTESIAN_POINT ( 'NONE',  ( 0.000000000000000000, 0.000000000000000000, -2.000000000000000000 ) ) ;
#1721 = CIRCLE ( 'NONE', #5688, 56.24900000005625600 ) ;
#1722 = DIRECTION ( 'NONE',  ( 1.000000000000000000, -0.000000000000000000, 0.000000000000000000 ) ) ;
#1723 = VERTEX_POINT ( 'NONE', #5352 ) ;
#1724 = DIRECTION ( 'NONE',  ( 0.000000000000000000, 0.000000000000000000, 1.000000000000000000 ) ) ;
#1725 = ORIENTED_EDGE ( 'NONE', *, *, #6339, .F. ) ;
#1726 = AXIS2_PLACEMENT_3D ( 'NONE', #18666, #5615, #11422 ) ;
#1727 = EDGE_CURVE ( 'NONE', #12710, #10680, #11505, .T. ) ;
#1728 = CARTESIAN_POINT ( 'NONE',  ( -3.333333333333335258, 2.694301256218251783, -3.300726591567079815 ) ) ;
#1729 = ORIENTED_EDGE ( 'NONE', *, *, #8148, .T. ) ;
#1730 = CIRCLE ( 'NONE', #16338, 24.00000000002399503 ) ;
#1731 = CIRCLE ( 'NONE', #6605, 24.00000000002399858 ) ;
#1732 = CONTEXT_DEPENDENT_SHAPE_REPRESENTATION ( #7081, #6166 ) ;
#1733 = ADVANCED_FACE ( 'NONE', ( #8318 ), #1760, .T. ) ;
#1734 = VERTEX_POINT ( 'NONE', #15461 ) ;
#1735 = ORIENTED_EDGE ( 'NONE', *, *, #824, .F. ) ;
#1736 = CIRCLE ( 'NONE', #13603, 26.24900000002624978 ) ;
#1737 = EDGE_LOOP ( 'NONE', ( #6979, #13598, #3643, #15086 ) ) ;
#1738 = FACE_OUTER_BOUND ( 'NONE', #1758, .T. ) ;
#1739 = CARTESIAN_POINT ( 'NONE',  ( 10.04305231718605285, -26.50000000000000000, -30.90933677959240811 ) ) ;
#1740 = VECTOR ( 'NONE', #534, 1000.000000000000000 ) ;
#1741 = AXIS2_PLACEMENT_3D ( 'NONE', #10000, #3504, #8070 ) ;
#1742 = CARTESIAN_POINT ( 'NONE',  ( -5.032868406504333869, -28.36021363089093938, 0.000000000000000000 ) ) ;
#1743 = DIRECTION ( 'NONE',  ( -0.000000000000000000, -1.000000000000000000, -0.000000000000000000 ) ) ;
#1744 = LINE ( 'NONE', #136, #12073 ) ;
#1745 = PLANE ( 'NONE',  #16514 ) ;
#1746 = CARTESIAN_POINT ( 'NONE',  ( 10.00000000000000000, 0.000000000000000000, 0.000000000000000000 ) ) ;
#1747 = DIRECTION ( 'NONE',  ( 0.1586811557617576196, -1.606889522083438452E-16, 0.9873298794253686506 ) ) ;
#1748 = ORIENTED_EDGE ( 'NONE', *, *, #2896, .F. ) ;
#1749 = FACE_OUTER_BOUND ( 'NONE', #11560, .T. ) ;
#1750 = CARTESIAN_POINT ( 'NONE',  ( 1.391697335622810172, 4.043246145443375461, -3.503898532754365913 ) ) ;
#1751 = CARTESIAN_POINT ( 'NONE',  ( 10.00000000000000000, 9.514709542736897063, 24.46385708179987262 ) ) ;
#1752 = AXIS2_PLACEMENT_3D ( 'NONE', #17869, #13494, #7758 ) ;
#1753 = ORIENTED_EDGE ( 'NONE', *, *, #3346, .T. ) ;
#1754 = ORIENTED_EDGE ( 'NONE', *, *, #3307, .T. ) ;
#1755 = CARTESIAN_POINT ( 'NONE',  ( 2.500000000000000000, 1.178949249685217415, 2.041999999999998483 ) ) ;
#1756 = DIRECTION ( 'NONE',  ( -2.031314180040287722E-16, -1.000000000000000000, -1.301042606982602609E-16 ) ) ;
#1757 = DIRECTION ( 'NONE',  ( 1.000000000000000000, 0.000000000000000000, -0.000000000000000000 ) ) ;
#1758 = EDGE_LOOP ( 'NONE', ( #16142, #8598, #12894, #6927 ) ) ;
#1759 = CIRCLE ( 'NONE', #11195, 24.00000000002399148 ) ;
#1760 = TOROIDAL_SURFACE ( 'NONE', #16357, 4.000000000000000000, 0.2500000000000000000 ) ;
#1761 = PRODUCT_DEFINITION_SHAPE ( 'NONE', 'NONE',  #8863 ) ;
#1762 = CARTESIAN_POINT ( 'NONE',  ( 4.078421086530217288, -3.990950201428958621, -1.000000000000000000 ) ) ;
#1763 = CARTESIAN_POINT ( 'NONE',  ( 1.250000000000000000, -6.429618962271402616, -1.000000000000000000 ) ) ;
#1764 = CIRCLE ( 'NONE', #16379, 5.000000000000004441 ) ;
#1765 = CARTESIAN_POINT ( 'NONE',  ( 0.000000000000000000, 3.000000000000000000, 0.000000000000000000 ) ) ;
#1766 = ORIENTED_EDGE ( 'NONE', *, *, #9354, .T. ) ;
#1767 = ADVANCED_FACE ( 'NONE', ( #15350 ), #18219, .F. ) ;
#1768 = CARTESIAN_POINT ( 'NONE',  ( -12.69999999999999929, 3.306546357697854128E-15, 27.00000000000000355 ) ) ;
#1769 = VECTOR ( 'NONE', #6486, 1000.000000000000227 ) ;
#1770 = SHAPE_REPRESENTATION ( 'motor', ( #8017 ), #16855 ) ;
#1771 = EDGE_CURVE ( 'NONE', #6586, #2692, #8142, .T. ) ;
#1772 = CIRCLE ( 'NONE', #8168, 25.00000000000000000 ) ;
#1773 = ORIENTED_EDGE ( 'NONE', *, *, #3966, .T. ) ;
#1774 = AXIS2_PLACEMENT_3D ( 'NONE', #18003, #10849, #14876 ) ;
#1775 = LINE ( 'NONE', #6150, #565 ) ;
#1776 = ORIENTED_EDGE ( 'NONE', *, *, #1609, .T. ) ;
#1777 = EDGE_CURVE ( 'NONE', #3205, #1351, #18794, .T. ) ;
#1778 = DIRECTION ( 'NONE',  ( -1.000000000000000000, -0.000000000000000000, 0.000000000000000000 ) ) ;
#1779 = EDGE_LOOP ( 'NONE', ( #16032, #2338, #6206, #546 ) ) ;
#1780 = ORIENTED_EDGE ( 'NONE', *, *, #11249, .F. ) ;
#1781 = CARTESIAN_POINT ( 'NONE',  ( 10.00000000000000000, 0.000000000000000000, 0.000000000000000000 ) ) ;
#1782 =( NAMED_UNIT ( * ) SI_UNIT ( $, .STERADIAN. ) SOLID_ANGLE_UNIT ( ) );
#1783 = EDGE_CURVE ( 'NONE', #19, #11318, #4212, .T. ) ;
#1784 = VERTEX_POINT ( 'NONE', #989 ) ;
#1785 = CYLINDRICAL_SURFACE ( 'NONE', #8196, 2.649999999999992806 ) ;
#1786 = CIRCLE ( 'NONE', #5129, 26.24900000002624978 ) ;
#1787 = EDGE_CURVE ( 'NONE', #9218, #9749, #16993, .T. ) ;
#1788 = VECTOR ( 'NONE', #11330, 1000.000000000000114 ) ;
#1789 = CIRCLE ( 'NONE', #7867, 12.00000000001200107 ) ;
#1790 = CARTESIAN_POINT ( 'NONE',  ( 10.00000000000000000, -56.23315539212689629, -1.335003989222221410 ) ) ;
#1791 = EDGE_LOOP ( 'NONE', ( #6997, #7591, #14174, #14685 ) ) ;
#1792 = EDGE_CURVE ( 'NONE', #10035, #1893, #8740, .T. ) ;
#1793 = EDGE_CURVE ( 'NONE', #12173, #10035, #8405, .T. ) ;
#1794 = AXIS2_PLACEMENT_3D ( 'NONE', #6987, #12798, #18601 ) ;
#1795 = ORIENTED_EDGE ( 'NONE', *, *, #8008, .F. ) ;
#1796 = LINE ( 'NONE', #277, #17542 ) ;
#1797 = DIRECTION ( 'NONE',  ( 0.000000000000000000, 0.000000000000000000, -1.000000000000000000 ) ) ;
#1798 = CARTESIAN_POINT ( 'NONE',  ( -4.197393957002303999, -7.773935952363655451E-14, -3.503767560748929810 ) ) ;
#1799 = ORIENTED_EDGE ( 'NONE', *, *, #964, .F. ) ;
#1800 = DIRECTION ( 'NONE',  ( 0.000000000000000000, 0.000000000000000000, 1.000000000000000000 ) ) ;
#1801 = EDGE_CURVE ( 'NONE', #3758, #1187, #18490, .T. ) ;
#1802 = PLANE ( 'NONE',  #11541 ) ;
#1803 = DIRECTION ( 'NONE',  ( 0.000000000000000000, 0.000000000000000000, 1.000000000000000000 ) ) ;
#1804 = DIRECTION ( 'NONE',  ( 0.000000000000000000, 0.000000000000000000, 1.000000000000000000 ) ) ;
#1805 = VERTEX_POINT ( 'NONE', #16206 ) ;
#1806 = LINE ( 'NONE', #8848, #5151 ) ;
#1807 = EDGE_CURVE ( 'NONE', #15635, #9576, #6637, .T. ) ;
#1808 = SURFACE_STYLE_USAGE ( .BOTH. , #10742 ) ;
#1809 = ORIENTED_EDGE ( 'NONE', *, *, #18302, .T. ) ;
#1810 = DIRECTION ( 'NONE',  ( -1.000000000000000000, 0.000000000000000000, 0.000000000000000000 ) ) ;
#1811 = DIRECTION ( 'NONE',  ( 0.000000000000000000, -1.000000000000000000, 0.000000000000000000 ) ) ;
#1812 = AXIS2_PLACEMENT_3D ( 'NONE', #3869, #12083, #13518 ) ;
#1813 = AXIS2_PLACEMENT_3D ( 'NONE', #3741, #9640, #6314 ) ;
#1814 = ORIENTED_EDGE ( 'NONE', *, *, #669, .F. ) ;
#1815 = CARTESIAN_POINT ( 'NONE',  ( -6.080745460913608902, 0.5192545390863924082, -1.000000000000000000 ) ) ;
#1816 = CYLINDRICAL_SURFACE ( 'NONE', #2469, 2.649999999999992806 ) ;
#1817 = ORIENTED_EDGE ( 'NONE', *, *, #16635, .T. ) ;
#1818 = PRESENTATION_STYLE_ASSIGNMENT (( #7807 ) ) ;
#1819 = FACE_BOUND ( 'NONE', #13502, .T. ) ;
#1820 = CYLINDRICAL_SURFACE ( 'NONE', #8160, 30.39999999999999858 ) ;
#1821 = AXIS2_PLACEMENT_3D ( 'NONE', #7093, #17200, #1483 ) ;
#1822 = DIRECTION ( 'NONE',  ( 0.000000000000000000, 0.000000000000000000, 1.000000000000000000 ) ) ;
#1823 = CARTESIAN_POINT ( 'NONE',  ( -4.888507282057958037, -29.45674523562211888, -2.000000000000000000 ) ) ;
#1824 = EDGE_LOOP ( 'NONE', ( #12807, #16818, #6158, #5332 ) ) ;
#1825 = DIRECTION ( 'NONE',  ( 0.000000000000000000, 0.000000000000000000, 1.000000000000000000 ) ) ;
#1826 = VERTEX_POINT ( 'NONE', #15925 ) ;
#1827 = EDGE_CURVE ( 'NONE', #8389, #18189, #16667, .T. ) ;
#1828 = DIRECTION ( 'NONE',  ( 0.000000000000000000, 0.000000000000000000, 1.000000000000000000 ) ) ;
#1829 = DIRECTION ( 'NONE',  ( 0.000000000000000000, -0.1564344650402382242, 0.9876883405951366601 ) ) ;
#1830 = ORIENTED_EDGE ( 'NONE', *, *, #2896, .T. ) ;
#1831 = ITEM_DEFINED_TRANSFORMATION ( 'NONE', 'NONE', #7137,  #8017 ) ;
#1832 = ORIENTED_EDGE ( 'NONE', *, *, #7124, .T. ) ;
#1833 = EDGE_LOOP ( 'NONE', ( #14175, #1300 ) ) ;
#1834 = ORIENTED_EDGE ( 'NONE', *, *, #14611, .F. ) ;
#1835 = CIRCLE ( 'NONE', #3365, 24.00000000002399858 ) ;
#1836 = LINE ( 'NONE', #14981, #15092 ) ;
#1837 = FILL_AREA_STYLE_COLOUR ( '', #4881 ) ;
#1838 = CYLINDRICAL_SURFACE ( 'NONE', #14238, 2.649999999999999467 ) ;
#1839 = CARTESIAN_POINT ( 'NONE',  ( 10.00000000000000000, 41.62350880771986539, -47.29147401531911754 ) ) ;
#1840 = CARTESIAN_POINT ( 'NONE',  ( 11.24999999999999645, 0.000000000000000000, 0.000000000000000000 ) ) ;
#1841 = DIRECTION ( 'NONE',  ( 0.1416665029469836024, 0.000000000000000000, 0.9899144417285627995 ) ) ;
#1842 = DIRECTION ( 'NONE',  ( -1.000000000000000000, -0.000000000000000000, -0.000000000000000000 ) ) ;
#1843 = CARTESIAN_POINT ( 'NONE',  ( 10.00000000000000000, -40.19788616105573453, -48.50907078259425731 ) ) ;
#1844 = ORIENTED_EDGE ( 'NONE', *, *, #15943, .F. ) ;
#1845 = EDGE_CURVE ( 'NONE', #1507, #12191, #2986, .T. ) ;
#1846 = CARTESIAN_POINT ( 'NONE',  ( 10.00000000000000000, -46.20417134726108088, -32.31183295104820985 ) ) ;
#1847 = FACE_OUTER_BOUND ( 'NONE', #14781, .T. ) ;
#1848 = CARTESIAN_POINT ( 'NONE',  ( 10.00000000000000000, 0.000000000000000000, 0.000000000000000000 ) ) ;
#1849 = ORIENTED_EDGE ( 'NONE', *, *, #7423, .T. ) ;
#1850 = ORIENTED_EDGE ( 'NONE', *, *, #9763, .F. ) ;
#1851 = CARTESIAN_POINT ( 'NONE',  ( 27.29487558977753991, 1.305124410222461284, -2.000000000000000000 ) ) ;
#1852 = VECTOR ( 'NONE', #18637, 1000.000000000000000 ) ;
#1853 = CARTESIAN_POINT ( 'NONE',  ( 0.000000000000000000, 13.24999999999999467, 0.000000000000000000 ) ) ;
#1854 = DIRECTION ( 'NONE',  ( 0.000000000000000000, 0.000000000000000000, 1.000000000000000000 ) ) ;
#1855 = ORIENTED_EDGE ( 'NONE', *, *, #11917, .F. ) ;
#1856 = EDGE_CURVE ( 'NONE', #4661, #17469, #8681, .T. ) ;
#1857 = DIRECTION ( 'NONE',  ( -1.000000000000000000, 0.000000000000000000, 0.000000000000000000 ) ) ;
#1858 = CARTESIAN_POINT ( 'NONE',  ( -0.1750025118121544265, -4.719839900820635314, -3.469254087858253399 ) ) ;
#1859 = DIRECTION ( 'NONE',  ( -0.000000000000000000, -1.000000000000000000, -0.000000000000000000 ) ) ;
#1860 = ORIENTED_EDGE ( 'NONE', *, *, #9882, .F. ) ;
#1862 = CARTESIAN_POINT ( 'NONE',  ( 10.00000000000000000, -50.71018745830427576, -24.33982105418956010 ) ) ;
#1861 = CIRCLE ( 'NONE', #4307, 63.00000000006298961 ) ;
#1863 = EDGE_CURVE ( 'NONE', #7974, #5783, #14590, .T. ) ;
#1864 = VERTEX_POINT ( 'NONE', #14317 ) ;
#1865 = CARTESIAN_POINT ( 'NONE',  ( 10.00000000000000000, 0.000000000000000000, 0.000000000000000000 ) ) ;
#1866 = ORIENTED_EDGE ( 'NONE', *, *, #6568, .F. ) ;
#1867 = AXIS2_PLACEMENT_3D ( 'NONE', #14318, #14592, #8682 ) ;
#1868 = LINE ( 'NONE', #16163, #9313 ) ;
#1869 = FACE_OUTER_BOUND ( 'NONE', #5848, .T. ) ;
#1870 = EDGE_LOOP ( 'NONE', ( #9986, #7665, #15841, #9983 ) ) ;
#1871 = VERTEX_POINT ( 'NONE', #2981 ) ;
#1872 = CARTESIAN_POINT ( 'NONE',  ( -87.43997332177200121, -14.11572627500821042, 6.475821446449874230 ) ) ;
#1873 = EDGE_LOOP ( 'NONE', ( #7692, #16429, #13707, #86 ) ) ;
#1874 = DIRECTION ( 'NONE',  ( 0.000000000000000000, 0.000000000000000000, 1.000000000000000000 ) ) ;
#1875 = EDGE_CURVE ( 'NONE', #3186, #11692, #14402, .T. ) ;
#1876 = CONICAL_SURFACE ( 'NONE', #17394, 4.000000000000000000, 0.8911886515913786111 ) ;
#1877 = PRODUCT_RELATED_PRODUCT_CATEGORY ( 'part', '', ( #11327 ) ) ;
#1878 = FACE_OUTER_BOUND ( 'NONE', #15547, .T. ) ;
#1879 = VERTEX_POINT ( 'NONE', #1361 ) ;
#1880 = VERTEX_POINT ( 'NONE', #17274 ) ;
#1881 = CARTESIAN_POINT ( 'NONE',  ( -5.032868406504333869, -28.36021363089093938, 0.000000000000000000 ) ) ;
#1882 = CARTESIAN_POINT ( 'NONE',  ( 130.0000000000000000, -34.99999999999999289, 125.0000000000000000 ) ) ;
#1883 = CYLINDRICAL_SURFACE ( 'NONE', #4798, 24.00000000002399858 ) ;
#1884 = ORIENTED_EDGE ( 'NONE', *, *, #7990, .F. ) ;
#1885 = LINE ( 'NONE', #10735, #13920 ) ;
#1886 = DIRECTION ( 'NONE',  ( 0.000000000000000000, -0.4539904997395351471, -0.8910065241883737830 ) ) ;
#1887 = DIRECTION ( 'NONE',  ( 0.000000000000000000, 0.000000000000000000, 1.000000000000000000 ) ) ;
#1888 = DIRECTION ( 'NONE',  ( 1.000000000000000000, 0.000000000000000000, 0.000000000000000000 ) ) ;
#1889 = ORIENTED_EDGE ( 'NONE', *, *, #8091, .F. ) ;
#1890 = DIRECTION ( 'NONE',  ( 0.000000000000000000, 0.000000000000000000, 1.000000000000000000 ) ) ;
#1891 = SURFACE_STYLE_FILL_AREA ( #13341 ) ;
#1892 = CIRCLE ( 'NONE', #13151, 4.000000000000000000 ) ;
#1893 = VERTEX_POINT ( 'NONE', #3072 ) ;
#1894 = DIRECTION ( 'NONE',  ( -0.000000000000000000, -0.000000000000000000, -1.000000000000000000 ) ) ;
#1895 = DIRECTION ( 'NONE',  ( -1.000000000000000000, 0.000000000000000000, 0.000000000000000000 ) ) ;
#1896 = ADVANCED_FACE ( 'NONE', ( #11453 ), #16057, .T. ) ;
#1897 = EDGE_CURVE ( 'NONE', #11652, #6251, #5412, .T. ) ;
#1898 = EDGE_CURVE ( 'NONE', #11226, #15342, #11829, .T. ) ;
#1899 = ADVANCED_FACE ( 'NONE', ( #5744 ), #13164, .T. ) ;
#1900 = ORIENTED_EDGE ( 'NONE', *, *, #4923, .T. ) ;
#1901 = AXIS2_PLACEMENT_3D ( 'NONE', #17050, #952, #6747 ) ;
#1902 = CARTESIAN_POINT ( 'NONE',  ( -4.000000000000000000, -2.309401076758512694, -3.433295621305382461 ) ) ;
#1903 = AXIS2_PLACEMENT_3D ( 'NONE', #7837, #14987, #10413 ) ;
#1904 = EDGE_CURVE ( 'NONE', #9105, #364, #4396, .T. ) ;
#1905 = VERTEX_POINT ( 'NONE', #10025 ) ;
#1906 = VECTOR ( 'NONE', #18383, 1000.000000000000000 ) ;
#1907 = PLANE ( 'NONE',  #17911 ) ;
#1908 = DIRECTION ( 'NONE',  ( 0.000000000000000000, 0.000000000000000000, -1.000000000000000000 ) ) ;
#1909 = EDGE_CURVE ( 'NONE', #6825, #12049, #7067, .T. ) ;
#1910 = FACE_OUTER_BOUND ( 'NONE', #10213, .T. ) ;
#1911 = DIRECTION ( 'NONE',  ( 1.000000000000000000, 0.000000000000000000, 0.000000000000000000 ) ) ;
#1912 = CARTESIAN_POINT ( 'NONE',  ( 10.00000000000000000, 16.10733642026559309, -53.89344778774794520 ) ) ;
#1913 = ORIENTED_EDGE ( 'NONE', *, *, #8065, .T. ) ;
#1914 = CARTESIAN_POINT ( 'NONE',  ( 50.00005079999999680, 4.769696007084728073, 1.500000000000000000 ) ) ;
#1915 = ORIENTED_EDGE ( 'NONE', *, *, #7281, .F. ) ;
#1916 = PRODUCT_DEFINITION_SHAPE ( 'NONE', 'NONE',  #18848 ) ;
#1917 = FACE_OUTER_BOUND ( 'NONE', #17047, .T. ) ;
#1918 = EDGE_LOOP ( 'NONE', ( #392, #6607, #2504, #17630 ) ) ;
#1919 = ADVANCED_FACE ( 'NONE', ( #10204 ), #2787, .F. ) ;
#1920 = ITEM_DEFINED_TRANSFORMATION ( 'NONE', 'NONE', #4705,  #8017 ) ;
#1921 = CIRCLE ( 'NONE', #2522, 63.00000000006298961 ) ;
#1922 = ORIENTED_EDGE ( 'NONE', *, *, #13802, .T. ) ;
#1923 = CIRCLE ( 'NONE', #13489, 12.00000000001200284 ) ;
#1924 = ORIENTED_EDGE ( 'NONE', *, *, #7619, .F. ) ;
#1925 = EDGE_CURVE ( 'NONE', #9576, #1332, #11730, .T. ) ;
#1926 = ORIENTED_EDGE ( 'NONE', *, *, #12328, .F. ) ;
#1927 = DIRECTION ( 'NONE',  ( -1.000000000000000000, -0.000000000000000000, 0.000000000000000000 ) ) ;
#1928 = LINE ( 'NONE', #8882, #14841 ) ;
#1929 = LINE ( 'NONE', #7730, #2930 ) ;
#1930 = AXIS2_PLACEMENT_3D ( 'NONE', #236, #16513, #2130 ) ;
#1931 = CARTESIAN_POINT ( 'NONE',  ( -31.74999999999995737, 0.000000000000000000, 0.000000000000000000 ) ) ;
#1932 = CARTESIAN_POINT ( 'NONE',  ( -12.50000000000000533, 0.000000000000000000, 0.000000000000000000 ) ) ;
#1933 = CARTESIAN_POINT ( 'NONE',  ( 10.00000000000000000, 53.06836994729258805, -18.64666490672316712 ) ) ;
#1934 = ORIENTED_EDGE ( 'NONE', *, *, #16162, .T. ) ;
#1935 = CARTESIAN_POINT ( 'NONE',  ( 3.333333333333335702, -2.694301256218268215, -3.300726591567084256 ) ) ;
#1936 = EDGE_LOOP ( 'NONE', ( #17912, #8400, #3142, #14656 ) ) ;
#1937 = CARTESIAN_POINT ( 'NONE',  ( -36.40576474687271258, 10.00000000000000000, -29.10033635316118961 ) ) ;
#1938 = LINE ( 'NONE', #6417, #10148 ) ;
#1939 = DIRECTION ( 'NONE',  ( 0.000000000000000000, -1.000000000000000000, 0.000000000000000000 ) ) ;
#1940 = VERTEX_POINT ( 'NONE', #10308 ) ;
#1941 = ORIENTED_EDGE ( 'NONE', *, *, #8242, .T. ) ;
#1942 = CARTESIAN_POINT ( 'NONE',  ( 0.000000000000000000, 1.017308535513159695, -56.37237871411032586 ) ) ;
#1943 = DIRECTION ( 'NONE',  ( 6.123233995736766036E-17, -1.000000000000000000, 0.000000000000000000 ) ) ;
#1944 = DIRECTION ( 'NONE',  ( 0.9995004958639130965, 0.000000000000000000, 0.03160314490350068367 ) ) ;
#1945 = VERTEX_POINT ( 'NONE', #16115 ) ;
#1946 = EDGE_CURVE ( 'NONE', #5117, #18145, #14677, .T. ) ;
#1947 = FACE_BOUND ( 'NONE', #2837, .T. ) ;
#1948 = CARTESIAN_POINT ( 'NONE',  ( 0.000000000000000000, 0.000000000000000000, 0.000000000000000000 ) ) ;
#1949 = DIRECTION ( 'NONE',  ( -1.000000000000000000, 0.000000000000000000, -0.000000000000000000 ) ) ;
#1950 = EDGE_LOOP ( 'NONE', ( #1924, #2038, #16540, #17201 ) ) ;
#1951 = CARTESIAN_POINT ( 'NONE',  ( 3.679171394226031122, 2.494631558665830973, -0.3503314178412474389 ) ) ;
#1952 = ORIENTED_EDGE ( 'NONE', *, *, #3368, .T. ) ;
#1953 = UNCERTAINTY_MEASURE_WITH_UNIT (LENGTH_MEASURE( 1.000000000000000082E-05 ), #4222, 'distance_accuracy_value', 'NONE');
#1954 = DIRECTION ( 'NONE',  ( 0.000000000000000000, 0.000000000000000000, 1.000000000000000000 ) ) ;
#1955 = ORIENTED_EDGE ( 'NONE', *, *, #5164, .T. ) ;
#1956 =( REPRESENTATION_RELATIONSHIP ('NONE','NONE', #11014, #434 ) REPRESENTATION_RELATIONSHIP_WITH_TRANSFORMATION ( #10402 )SHAPE_REPRESENTATION_RELATIONSHIP( ) );
#1957 = STYLED_ITEM ( 'NONE', ( #14929 ), #6260 ) ;
#1958 = DIRECTION ( 'NONE',  ( 0.000000000000000000, 0.000000000000000000, 1.000000000000000000 ) ) ;
#1959 = CARTESIAN_POINT ( 'NONE',  ( -0.6640947660597427138, 4.471078309994878985, -3.602146406945963442 ) ) ;
#1960 = VERTEX_POINT ( 'NONE', #18096 ) ;
#1961 = EDGE_LOOP ( 'NONE', ( #2882, #3153, #16697, #4559 ) ) ;
#1962 = ADVANCED_FACE ( 'NONE', ( #9052 ), #4953, .T. ) ;
#1963 = CARTESIAN_POINT ( 'NONE',  ( -36.40576474687271258, 10.00000000000000000, -29.10033635316118961 ) ) ;
#1964 = FILL_AREA_STYLE ('',( #7964 ) ) ;
#1965 = VERTEX_POINT ( 'NONE', #14767 ) ;
#1966 = DIRECTION ( 'NONE',  ( -0.000000000000000000, 1.000000000000000000, -0.000000000000000000 ) ) ;
#1967 = EDGE_CURVE ( 'NONE', #9230, #13703, #12285, .T. ) ;
#1968 = AXIS2_PLACEMENT_3D ( 'NONE', #16431, #9269, #9371 ) ;
#1969 = CARTESIAN_POINT ( 'NONE',  ( -10.00000000000000000, -26.45033635316118747, 33.75576474687270689 ) ) ;
#1970 = VECTOR ( 'NONE', #14156, 1000.000000000000000 ) ;
#1971 = AXIS2_PLACEMENT_3D ( 'NONE', #11706, #4557, #7409 ) ;
#1972 = ORIENTED_EDGE ( 'NONE', *, *, #9121, .T. ) ;
#1973 = ORIENTED_EDGE ( 'NONE', *, *, #3716, .T. ) ;
#1974 = CARTESIAN_POINT ( 'NONE',  ( 20.55500000000001748, 0.000000000000000000, 0.000000000000000000 ) ) ;
#1975 = DIRECTION ( 'NONE',  ( 0.000000000000000000, 0.3090169943749410120, 0.9510565162951556406 ) ) ;
#1976 = FACE_OUTER_BOUND ( 'NONE', #7216, .T. ) ;
#1977 = ORIENTED_EDGE ( 'NONE', *, *, #10728, .F. ) ;
#1978 = DIRECTION ( 'NONE',  ( -1.000000000000000000, -0.000000000000000000, -0.000000000000000000 ) ) ;
#1979 = DIRECTION ( 'NONE',  ( 0.000000000000000000, 0.000000000000000000, 1.000000000000000000 ) ) ;
#1980 = DIRECTION ( 'NONE',  ( -1.000000000000000000, -0.000000000000000000, -0.000000000000000000 ) ) ;
#1981 = CARTESIAN_POINT ( 'NONE',  ( 45.00000000000000000, 10.00000000000000000, -2.650000000000511946 ) ) ;
#1982 = ORIENTED_EDGE ( 'NONE', *, *, #15760, .F. ) ;
#1983 = PLANE ( 'NONE',  #16615 ) ;
#1984 = CARTESIAN_POINT ( 'NONE',  ( 10.00000000000000000, 0.000000000000000000, 0.000000000000000000 ) ) ;
#1985 = AXIS2_PLACEMENT_3D ( 'NONE', #5269, #6614, #16805 ) ;
#1986 = ORIENTED_EDGE ( 'NONE', *, *, #11152, .F. ) ;
#1987 = CYLINDRICAL_SURFACE ( 'NONE', #13662, 4.250000000000000000 ) ;
#1988 = DIRECTION ( 'NONE',  ( -0.000000000000000000, -1.000000000000000000, -0.000000000000000000 ) ) ;
#1989 = AXIS2_PLACEMENT_3D ( 'NONE', #13677, #7858, #6427 ) ;
#1990 = AXIS2_PLACEMENT_3D ( 'NONE', #6317, #3744, #9645 ) ;
#1991 = AXIS2_PLACEMENT_3D ( 'NONE', #7672, #14832, #13501 ) ;
#1992 = VECTOR ( 'NONE', #16512, 1000.000000000000000 ) ;
#1993 = ORIENTED_EDGE ( 'NONE', *, *, #14984, .T. ) ;
#1994 = CARTESIAN_POINT ( 'NONE',  ( 10.00000000000000000, 38.81885513160045065, -40.70683587897917022 ) ) ;
#1995 = CIRCLE ( 'NONE', #7772, 26.24900000002625333 ) ;
#1996 = EDGE_LOOP ( 'NONE', ( #7930, #18641, #8266, #16907 ) ) ;
#1997 = SURFACE_STYLE_FILL_AREA ( #11991 ) ;
#1998 = AXIS2_PLACEMENT_3D ( 'NONE', #9837, #14222, #1184 ) ;
#1999 = DIRECTION ( 'NONE',  ( 1.000000000000000000, 0.000000000000000000, -0.000000000000000000 ) ) ;
#2000 = ADVANCED_FACE ( 'NONE', ( #13726 ), #10472, .T. ) ;
#2001 = EDGE_CURVE ( 'NONE', #9477, #13093, #2002, .T. ) ;
#2002 = LINE ( 'NONE', #4864, #5114 ) ;
#2003 = CARTESIAN_POINT ( 'NONE',  ( -10.00000000000000000, 0.000000000000000000, 0.000000000000000000 ) ) ;
#2004 = DIRECTION ( 'NONE',  ( -0.000000000000000000, 1.000000000000000000, -0.000000000000000000 ) ) ;
#2005 = EDGE_LOOP ( 'NONE', ( #7388, #9322, #8554, #8360 ) ) ;
#2006 = CARTESIAN_POINT ( 'NONE',  ( 0.000000000000000000, -20.32630374611172641, -16.60877409751190470 ) ) ;
#2007 = EDGE_CURVE ( 'NONE', #9233, #7319, #3303, .T. ) ;
#2008 = CARTESIAN_POINT ( 'NONE',  ( 0.000000000000000000, 0.000000000000000000, 0.000000000000000000 ) ) ;
#2009 = EDGE_LOOP ( 'NONE', ( #17323, #14040, #14167, #14688 ) ) ;
#2010 = AXIS2_PLACEMENT_3D ( 'NONE', #5080, #9754, #9655 ) ;
#2011 = CIRCLE ( 'NONE', #9930, 12.00000000001200817 ) ;
#2012 = CONTEXT_DEPENDENT_SHAPE_REPRESENTATION ( #13900, #2989 ) ;
#2013 = ADVANCED_FACE ( 'NONE', ( #3443 ), #15158, .T. ) ;
#2014 = CIRCLE ( 'NONE', #14479, 24.00000000002399858 ) ;
#2015 = VERTEX_POINT ( 'NONE', #4674 ) ;
#2016 = AXIS2_PLACEMENT_3D ( 'NONE', #7448, #14891, #17655 ) ;
#2017 = AXIS2_PLACEMENT_3D ( 'NONE', #2176, #758, #3339 ) ;
#2018 = EDGE_LOOP ( 'NONE', ( #15909, #13072, #16843, #3478 ) ) ;
#2019 = EDGE_CURVE ( 'NONE', #5476, #6010, #306, .T. ) ;
#2020 = ORIENTED_EDGE ( 'NONE', *, *, #16871, .F. ) ;
#2021 = DIRECTION ( 'NONE',  ( 0.000000000000000000, 0.000000000000000000, 1.000000000000000000 ) ) ;
#2022 = CARTESIAN_POINT ( 'NONE',  ( 2.500000000000000000, 2.357898499370432166, -2.385244779468109755E-15 ) ) ;
#2023 = AXIS2_PLACEMENT_3D ( 'NONE', #11529, #10177, #14294 ) ;
#2024 = AXIS2_PLACEMENT_3D ( 'NONE', #107, #7136, #11715 ) ;
#2025 = DIRECTION ( 'NONE',  ( -1.000000000000000000, -0.000000000000000000, -0.000000000000000000 ) ) ;
#2026 = CARTESIAN_POINT ( 'NONE',  ( 0.000000000000000000, 39.14194549634364506, 40.58063702438359144 ) ) ;
#2027 = ADVANCED_FACE ( 'NONE', ( #13633 ), #585, .T. ) ;
#2029 = DIRECTION ( 'NONE',  ( -1.000000000000000000, -0.000000000000000000, -0.000000000000000000 ) ) ;
#2028 = AXIS2_PLACEMENT_3D ( 'NONE', #7255, #13074, #10203 ) ;
#2030 = ADVANCED_FACE ( 'NONE', ( #6390 ), #7533, .T. ) ;
#2031 = DIRECTION ( 'NONE',  ( -1.000000000000000000, 0.000000000000000000, -0.000000000000000000 ) ) ;
#2032 = DIRECTION ( 'NONE',  ( 0.000000000000000000, 0.000000000000000000, 1.000000000000000000 ) ) ;
#2033 = AXIS2_PLACEMENT_3D ( 'NONE', #1220, #12453, #13874 ) ;
#2034 = LINE ( 'NONE', #6412, #15369 ) ;
#2035 = ORIENTED_EDGE ( 'NONE', *, *, #747, .T. ) ;
#2036 = AXIS2_PLACEMENT_3D ( 'NONE', #7128, #15817, #2670 ) ;
#2037 = CYLINDRICAL_SURFACE ( 'NONE', #18207, 12.00000000001200817 ) ;
#2038 = ORIENTED_EDGE ( 'NONE', *, *, #11988, .F. ) ;
#2039 = DIRECTION ( 'NONE',  ( -0.000000000000000000, 1.000000000000000000, -0.000000000000000000 ) ) ;
#2040 = CYLINDRICAL_SURFACE ( 'NONE', #7098, 24.00000000002399858 ) ;
#2041 = CARTESIAN_POINT ( 'NONE',  ( 10.00000000000000000, -7.478235706488566059, -55.74967257055892134 ) ) ;
#2042 = ORIENTED_EDGE ( 'NONE', *, *, #16122, .F. ) ;
#2043 = ORIENTED_EDGE ( 'NONE', *, *, #8293, .T. ) ;
#2044 = ADVANCED_FACE ( 'NONE', ( #15055 ), #1820, .T. ) ;
#2045 = DIRECTION ( 'NONE',  ( -0.000000000000000000, 1.000000000000000000, -0.000000000000000000 ) ) ;
#2046 = CARTESIAN_POINT ( 'NONE',  ( -56.50000000009000445, -25.00000000000000000, 3.817814120399276590E-13 ) ) ;
#2047 = CARTESIAN_POINT ( 'NONE',  ( 0.000000000000000000, 23.88582760061481380, 22.76987570971536101 ) ) ;
#2048 = ORIENTED_EDGE ( 'NONE', *, *, #10295, .T. ) ;
#2049 = CIRCLE ( 'NONE', #11777, 56.24900000005625600 ) ;
#2050 = AXIS2_PLACEMENT_3D ( 'NONE', #15904, #11709, #2953 ) ;
#2051 = AXIS2_PLACEMENT_3D ( 'NONE', #7297, #5869, #8721 ) ;
#2052 = VECTOR ( 'NONE', #11216, 1000.000000000000000 ) ;
#2053 = DIRECTION ( 'NONE',  ( -1.000000000000000000, -0.000000000000000000, -0.000000000000000000 ) ) ;
#2054 = DIRECTION ( 'NONE',  ( 0.000000000000000000, 0.000000000000000000, 1.000000000000000000 ) ) ;
#2055 = CARTESIAN_POINT ( 'NONE',  ( 5.000000000000000000, -14.27431201565546459, 29.75305054077467659 ) ) ;
#2056 = ORIENTED_EDGE ( 'NONE', *, *, #17418, .T. ) ;
#2057 = LINE ( 'NONE', #3485, #10083 ) ;
#2058 = AXIS2_PLACEMENT_3D ( 'NONE', #15507, #10926, #18170 ) ;
#2059 = VERTEX_POINT ( 'NONE', #7710 ) ;
#2060 = CARTESIAN_POINT ( 'NONE',  ( 10.00000000000000000, 55.33199130079800199, -10.11537145609316646 ) ) ;
#2061 = ORIENTED_EDGE ( 'NONE', *, *, #17397, .F. ) ;
#2062 = CIRCLE ( 'NONE', #7220, 33.00000000003299760 ) ;
#2063 = DIRECTION ( 'NONE',  ( 0.000000000000000000, 0.000000000000000000, 1.000000000000000000 ) ) ;
#2064 = CARTESIAN_POINT ( 'NONE',  ( 10.00000000000000000, -46.20417134726153563, 32.31183295104756326 ) ) ;
#2065 = AXIS2_PLACEMENT_3D ( 'NONE', #11479, #2894, #10046 ) ;
#2066 = ORIENTED_EDGE ( 'NONE', *, *, #12078, .T. ) ;
#2067 = ORIENTED_EDGE ( 'NONE', *, *, #7457, .F. ) ;
#2068 = AXIS2_PLACEMENT_3D ( 'NONE', #17088, #15644, #2591 ) ;
#2069 = ADVANCED_FACE ( 'NONE', ( #16678 ), #14967, .T. ) ;
#2070 = DIRECTION ( 'NONE',  ( 0.000000000000000000, 0.000000000000000000, 1.000000000000000000 ) ) ;
#2071 = ORIENTED_EDGE ( 'NONE', *, *, #2237, .F. ) ;
#2072 = LINE ( 'NONE', #7877, #12145 ) ;
#2073 = AXIS2_PLACEMENT_3D ( 'NONE', #6628, #12618, #2525 ) ;
#2074 = VECTOR ( 'NONE', #10954, 1000.000000000000000 ) ;
#2075 = CARTESIAN_POINT ( 'NONE',  ( 0.000000000000000000, 0.000000000000000000, 0.000000000000000000 ) ) ;
#2076 = VECTOR ( 'NONE', #14136, 1000.000000000000000 ) ;
#2077 = VECTOR ( 'NONE', #2768, 1000.000000000000000 ) ;
#2078 = ORIENTED_EDGE ( 'NONE', *, *, #14142, .T. ) ;
#2079 = ADVANCED_FACE ( 'NONE', ( #3250 ), #13448, .F. ) ;
#2080 = PRODUCT_DEFINITION_SHAPE ( 'NONE', 'NONE',  #18822 ) ;
#2081 = ORIENTED_EDGE ( 'NONE', *, *, #16874, .T. ) ;
#2082 = LINE ( 'NONE', #6544, #18168 ) ;
#2083 = LINE ( 'NONE', #12177, #15046 ) ;
#2084 = LINE ( 'NONE', #13330, #12691 ) ;
#2085 = VERTEX_POINT ( 'NONE', #17916 ) ;
#2086 = CYLINDRICAL_SURFACE ( 'NONE', #14218, 12.00000000001200817 ) ;
#2087 = EDGE_CURVE ( 'NONE', #7622, #417, #4221, .T. ) ;
#2088 = CARTESIAN_POINT ( 'NONE',  ( 3.680118525130245732, -2.494084732383344605, -0.3507732604232533524 ) ) ;
#2089 = CARTESIAN_POINT ( 'NONE',  ( -1.250000000000000000, -6.429618962271402616, -1.000000000000000000 ) ) ;
#2090 = VECTOR ( 'NONE', #1278, 1000.000000000000000 ) ;
#2091 = DIRECTION ( 'NONE',  ( 0.000000000000000000, 0.000000000000000000, 1.000000000000000000 ) ) ;
#2092 = ORIENTED_EDGE ( 'NONE', *, *, #3782, .F. ) ;
#2093 = CARTESIAN_POINT ( 'NONE',  ( 0.000000000000000000, 0.000000000000000000, 0.000000000000000000 ) ) ;
#2094 = ORIENTED_EDGE ( 'NONE', *, *, #1807, .F. ) ;
#2095 = DIRECTION ( 'NONE',  ( 0.000000000000000000, -0.5000000000000011102, -0.8660254037844379305 ) ) ;
#2096 = DIRECTION ( 'NONE',  ( 0.000000000000000000, 0.000000000000000000, 1.000000000000000000 ) ) ;
#2097 = AXIS2_PLACEMENT_3D ( 'NONE', #16593, #15458, #3830 ) ;
#2098 = CIRCLE ( 'NONE', #12144, 2.041999999999999815 ) ;
#2099 = ADVANCED_FACE ( 'NONE', ( #1910 ), #13533, .F. ) ;
#2100 = ORIENTED_EDGE ( 'NONE', *, *, #14263, .T. ) ;
#2101 = EDGE_LOOP ( 'NONE', ( #4438, #9725, #8083, #4707 ) ) ;
#2102 = DIRECTION ( 'NONE',  ( -0.000000000000000000, 1.000000000000000000, -0.000000000000000000 ) ) ;
#2103 = DIRECTION ( 'NONE',  ( -0.000000000000000000, 1.000000000000000000, -0.000000000000000000 ) ) ;
#2104 = CARTESIAN_POINT ( 'NONE',  ( 0.000000000000000000, 0.000000000000000000, -4.694516984716113228 ) ) ;
#2105 = CARTESIAN_POINT ( 'NONE',  ( -10.00000000000000000, 0.000000000000000000, 0.000000000000000000 ) ) ;
#2106 = DIRECTION ( 'NONE',  ( 0.000000000000000000, -1.224646799147330774E-16, 1.000000000000000000 ) ) ;
#2107 = VERTEX_POINT ( 'NONE', #967 ) ;
#2108 = CARTESIAN_POINT ( 'NONE',  ( 10.00000000000000000, 0.000000000000000000, 0.000000000000000000 ) ) ;
#2109 = DIRECTION ( 'NONE',  ( -1.000000000000000000, -0.000000000000000000, -0.000000000000000000 ) ) ;
#2110 = AXIS2_PLACEMENT_3D ( 'NONE', #11430, #2772, #2862 ) ;
#2111 = ORIENTED_EDGE ( 'NONE', *, *, #8088, .T. ) ;
#2112 = CIRCLE ( 'NONE', #2734, 26.24900000002625688 ) ;
#2113 = ORIENTED_EDGE ( 'NONE', *, *, #14019, .F. ) ;
#2114 = ADVANCED_FACE ( 'NONE', ( #18480 ), #15624, .T. ) ;
#2115 = EDGE_CURVE ( 'NONE', #2471, #280, #4810, .T. ) ;
#2116 = ORIENTED_EDGE ( 'NONE', *, *, #11100, .F. ) ;
#2117 = ORIENTED_EDGE ( 'NONE', *, *, #5553, .F. ) ;
#2118 = CARTESIAN_POINT ( 'NONE',  ( 0.000000000000000000, -5.120903701083534543E-13, -45.00000000000000000 ) ) ;
#2119 = PRODUCT_RELATED_PRODUCT_CATEGORY ( 'part', '', ( #17887 ) ) ;
#2120 = AXIS2_PLACEMENT_3D ( 'NONE', #59, #8439, #7184 ) ;
#2121 = CYLINDRICAL_SURFACE ( 'NONE', #16679, 150.0000000000000284 ) ;
#2122 = CYLINDRICAL_SURFACE ( 'NONE', #3242, 56.24900000005625600 ) ;
#2123 = DIRECTION ( 'NONE',  ( 0.000000000000000000, -1.000000000000000000, 0.000000000000000000 ) ) ;
#2124 = CARTESIAN_POINT ( 'NONE',  ( -90.67999921423555065, 1.000000000000018208, -4.751589320297106234 ) ) ;
#2125 = CARTESIAN_POINT ( 'NONE',  ( 10.00000000000000000, -31.97297851452457351, 46.27827401617392411 ) ) ;
#2126 = ORIENTED_EDGE ( 'NONE', *, *, #7213, .F. ) ;
#2127 = CARTESIAN_POINT ( 'NONE',  ( 10.00000000000000000, -26.45033635316118747, 39.05576474687271116 ) ) ;
#2128 = ORIENTED_EDGE ( 'NONE', *, *, #7354, .F. ) ;
#2129 = ADVANCED_FACE ( 'NONE', ( #13810 ), #11335, .T. ) ;
#2130 = DIRECTION ( 'NONE',  ( 0.000000000000000000, 0.000000000000000000, 1.000000000000000000 ) ) ;
#2131 = CARTESIAN_POINT ( 'NONE',  ( 0.000000000000000000, -13.75000000000000355, 27.50000000000000000 ) ) ;
#2132 = ORIENTED_EDGE ( 'NONE', *, *, #11827, .T. ) ;
#2133 = ORIENTED_EDGE ( 'NONE', *, *, #1273, .T. ) ;
#2134 = DIRECTION ( 'NONE',  ( 0.000000000000000000, -0.8660254037844390407, -0.4999999999999992784 ) ) ;
#2135 = DIRECTION ( 'NONE',  ( 0.000000000000000000, 0.000000000000000000, 1.000000000000000000 ) ) ;
#2136 = CARTESIAN_POINT ( 'NONE',  ( -4.211140560182196957, 2.431303136016537803, -3.745885042887433514 ) ) ;
#2137 = ORIENTED_EDGE ( 'NONE', *, *, #14327, .T. ) ;
#2138 = AXIS2_PLACEMENT_3D ( 'NONE', #11658, #8119, #10874 ) ;
#2139 = ADVANCED_FACE ( 'NONE', ( #3636 ), #17070, .F. ) ;
#2140 = MECHANICAL_DESIGN_GEOMETRIC_PRESENTATION_REPRESENTATION (  '', ( #622 ), #17654 ) ;
#2141 = EDGE_CURVE ( 'NONE', #14103, #1152, #2566, .T. ) ;
#2142 = DIRECTION ( 'NONE',  ( -0.000000000000000000, 1.000000000000000000, -0.000000000000000000 ) ) ;
#2143 = EDGE_CURVE ( 'NONE', #17667, #6907, #18287, .T. ) ;
#2144 = FACE_BOUND ( 'NONE', #18626, .T. ) ;
#2145 = DIRECTION ( 'NONE',  ( -1.000000000000000000, -0.000000000000000000, -0.000000000000000000 ) ) ;
#2146 = EDGE_CURVE ( 'NONE', #1162, #11016, #8385, .T. ) ;
#2147 = ORIENTED_EDGE ( 'NONE', *, *, #11094, .F. ) ;
#2148 = CARTESIAN_POINT ( 'NONE',  ( 0.000000000000000000, 0.000000000000000000, 0.000000000000000000 ) ) ;
#2149 = ORIENTED_EDGE ( 'NONE', *, *, #4870, .F. ) ;
#2150 = UNCERTAINTY_MEASURE_WITH_UNIT (LENGTH_MEASURE( 1.000000000000000082E-05 ), #3560, 'distance_accuracy_value', 'NONE');
#2151 = DIRECTION ( 'NONE',  ( 0.000000000000000000, 0.000000000000000000, -1.000000000000000000 ) ) ;
#2152 = VERTEX_POINT ( 'NONE', #12384 ) ;
#2153 = AXIS2_PLACEMENT_3D ( 'NONE', #4669, #7705, #4763 ) ;
#2154 = EDGE_CURVE ( 'NONE', #17009, #7434, #11138, .T. ) ;
#2155 = DIRECTION ( 'NONE',  ( 0.000000000000000000, 0.000000000000000000, -1.000000000000000000 ) ) ;
#2156 = DIRECTION ( 'NONE',  ( 1.000000000000000000, 0.000000000000000000, 0.000000000000000000 ) ) ;
#2157 = VERTEX_POINT ( 'NONE', #12773 ) ;
#2158 = ORIENTED_EDGE ( 'NONE', *, *, #18549, .T. ) ;
#2159 = DIRECTION ( 'NONE',  ( -1.000000000000000000, -0.000000000000000000, -0.000000000000000000 ) ) ;
#2160 = ORIENTED_EDGE ( 'NONE', *, *, #2665, .T. ) ;
#2161 = LINE ( 'NONE', #12448, #9732 ) ;
#2162 = EDGE_CURVE ( 'NONE', #8506, #1304, #16965, .T. ) ;
#2163 = CIRCLE ( 'NONE', #10382, 2.649999999999999467 ) ;
#2164 = DIRECTION ( 'NONE',  ( 0.000000000000000000, 0.000000000000000000, 1.000000000000000000 ) ) ;
#2165 = DIRECTION ( 'NONE',  ( 0.000000000000000000, 0.000000000000000000, 1.000000000000000000 ) ) ;
#2166 = EDGE_CURVE ( 'NONE', #2762, #3664, #12104, .T. ) ;
#2167 = ORIENTED_EDGE ( 'NONE', *, *, #15982, .T. ) ;
#2168 = ORIENTED_EDGE ( 'NONE', *, *, #11210, .F. ) ;
#2169 = CARTESIAN_POINT ( 'NONE',  ( 0.000000000000000000, 32.46095361140693569, 5.940243314904326333 ) ) ;
#2170 = DIRECTION ( 'NONE',  ( 0.000000000000000000, 0.000000000000000000, 1.000000000000000000 ) ) ;
#2171 = DIRECTION ( 'NONE',  ( 0.000000000000000000, 0.000000000000000000, 1.000000000000000000 ) ) ;
#2172 = ORIENTED_EDGE ( 'NONE', *, *, #13675, .T. ) ;
#2173 = DIRECTION ( 'NONE',  ( -0.000000000000000000, 1.000000000000000000, -0.000000000000000000 ) ) ;
#2174 = CARTESIAN_POINT ( 'NONE',  ( 2.595115354961440524, -7.673029147243177306, 0.000000000000000000 ) ) ;
#2175 = DIRECTION ( 'NONE',  ( -1.000000000000000000, 0.000000000000000000, 0.000000000000000000 ) ) ;
#2176 = CARTESIAN_POINT ( 'NONE',  ( 10.00000000000000000, -13.40641754777683126, 24.79895094899255170 ) ) ;
#2177 = ORIENTED_EDGE ( 'NONE', *, *, #12687, .F. ) ;
#2178 = CIRCLE ( 'NONE', #318, 63.00000000006298961 ) ;
#2179 = DIRECTION ( 'NONE',  ( 0.000000000000000000, 0.000000000000000000, 1.000000000000000000 ) ) ;
#2180 = ORIENTED_EDGE ( 'NONE', *, *, #11126, .F. ) ;
#2181 = LINE ( 'NONE', #16853, #17909 ) ;
#2182 = DIRECTION ( 'NONE',  ( 1.000000000000000000, 0.000000000000000000, 0.000000000000000000 ) ) ;
#2183 = AXIS2_PLACEMENT_3D ( 'NONE', #7432, #6107, #9053 ) ;
#2184 = CIRCLE ( 'NONE', #4619, 24.00000000002399858 ) ;
#2185 = EDGE_CURVE ( 'NONE', #16278, #4962, #6334, .T. ) ;
#2186 = ORIENTED_EDGE ( 'NONE', *, *, #4002, .F. ) ;
#2187 = ORIENTED_EDGE ( 'NONE', *, *, #16222, .F. ) ;
#2188 = DIRECTION ( 'NONE',  ( -0.000000000000000000, 1.000000000000000000, -0.000000000000000000 ) ) ;
#2189 = CARTESIAN_POINT ( 'NONE',  ( 3.999999999999999112, -0.7890432684750902093, -0.04868663549882291247 ) ) ;
#2190 = DIRECTION ( 'NONE',  ( 1.000000000000000000, 0.000000000000000000, 0.000000000000000000 ) ) ;
#2191 = LINE ( 'NONE', #584, #12991 ) ;
#2192 = VECTOR ( 'NONE', #4103, 1000.000000000000000 ) ;
#2193 = CARTESIAN_POINT ( 'NONE',  ( 9.345251662538453630, -28.92794965710190525, 0.000000000000000000 ) ) ;
#2194 = DIRECTION ( 'NONE',  ( -1.000000000000000000, -0.000000000000000000, -0.000000000000000000 ) ) ;
#2195 = ORIENTED_EDGE ( 'NONE', *, *, #12960, .T. ) ;
#2196 = FACE_OUTER_BOUND ( 'NONE', #163, .T. ) ;
#2197 = DIRECTION ( 'NONE',  ( -1.000000000000000000, 0.000000000000000000, 0.000000000000000000 ) ) ;
#2198 = ORIENTED_EDGE ( 'NONE', *, *, #5386, .T. ) ;
#2199 = EDGE_CURVE ( 'NONE', #10808, #1653, #6646, .T. ) ;
#2200 = CONTEXT_DEPENDENT_SHAPE_REPRESENTATION ( #11699, #16370 ) ;
#2201 = ORIENTED_EDGE ( 'NONE', *, *, #2863, .T. ) ;
#2202 = EDGE_CURVE ( 'NONE', #10253, #14080, #6024, .T. ) ;
#2203 = AXIS2_PLACEMENT_3D ( 'NONE', #81, #7110, #5961 ) ;
#2204 = ORIENTED_EDGE ( 'NONE', *, *, #4568, .F. ) ;
#2205 = VECTOR ( 'NONE', #8271, 1000.000000000000000 ) ;
#2206 = APPLICATION_CONTEXT ( 'automotive_design' ) ;
#2207 = ORIENTED_EDGE ( 'NONE', *, *, #17907, .F. ) ;
#2208 = CARTESIAN_POINT ( 'NONE',  ( 0.000000000000000000, 56.37237871411034007, 1.017308535512583711 ) ) ;
#2209 = PLANE ( 'NONE',  #7316 ) ;
#2210 =( LENGTH_UNIT ( ) NAMED_UNIT ( * ) SI_UNIT ( .MILLI., .METRE. ) );
#2211 = FACE_OUTER_BOUND ( 'NONE', #8833, .T. ) ;
#2212 = FACE_OUTER_BOUND ( 'NONE', #3227, .T. ) ;
#2213 = DIRECTION ( 'NONE',  ( 0.000000000000000000, 0.000000000000000000, -1.000000000000000000 ) ) ;
#2214 = DIRECTION ( 'NONE',  ( 0.000000000000000000, 0.000000000000000000, -1.000000000000000000 ) ) ;
#2215 = ORIENTED_EDGE ( 'NONE', *, *, #10265, .T. ) ;
#2216 = DIRECTION ( 'NONE',  ( 0.000000000000000000, 0.000000000000000000, 1.000000000000000000 ) ) ;
#2217 = ORIENTED_EDGE ( 'NONE', *, *, #198, .F. ) ;
#2218 = AXIS2_PLACEMENT_3D ( 'NONE', #9108, #9392, #12335 ) ;
#2219 = LINE ( 'NONE', #14037, #16226 ) ;
#2220 = FACE_OUTER_BOUND ( 'NONE', #5493, .T. ) ;
#2221 = EDGE_LOOP ( 'NONE', ( #14978, #848, #7614, #14276 ) ) ;
#2222 = VERTEX_POINT ( 'NONE', #3726 ) ;
#2223 = CLOSED_SHELL ( 'NONE', ( #15200, #17927, #1710, #5636, #4878, #2825, #17976, #16218, #14114, #15768, #13678, #3090, #12859, #4334, #4412, #8329, #14903, #1510, #9932 ) ) ;
#2224 = DIRECTION ( 'NONE',  ( 0.000000000000000000, 0.000000000000000000, 1.000000000000000000 ) ) ;
#2225 =( LENGTH_UNIT ( ) NAMED_UNIT ( * ) SI_UNIT ( .MILLI., .METRE. ) );
#2226 = DIRECTION ( 'NONE',  ( 0.000000000000000000, 0.000000000000000000, 1.000000000000000000 ) ) ;
#2227 = ORIENTED_EDGE ( 'NONE', *, *, #3683, .T. ) ;
#2228 = AXIS2_PLACEMENT_3D ( 'NONE', #5076, #11170, #17000 ) ;
#2229 = FACE_OUTER_BOUND ( 'NONE', #6165, .T. ) ;
#2230 = CARTESIAN_POINT ( 'NONE',  ( 0.000000000000000000, 15.00000000000000000, 20.00000000000000000 ) ) ;
#2231 = LINE ( 'NONE', #11283, #2076 ) ;
#2232 = ORIENTED_EDGE ( 'NONE', *, *, #12399, .T. ) ;
#2233 = CYLINDRICAL_SURFACE ( 'NONE', #55, 27.50000000000000000 ) ;
#2234 = ORIENTED_EDGE ( 'NONE', *, *, #6922, .F. ) ;
#2235 = CARTESIAN_POINT ( 'NONE',  ( 0.000000000000000000, 26.49895292618076326, -49.76630880786279931 ) ) ;
#2236 = ORIENTED_EDGE ( 'NONE', *, *, #7658, .F. ) ;
#2237 = EDGE_CURVE ( 'NONE', #15264, #16644, #9523, .T. ) ;
#2238 = EDGE_CURVE ( 'NONE', #13691, #9705, #13915, .T. ) ;
#2239 = ADVANCED_FACE ( 'NONE', ( #11041 ), #16863, .F. ) ;
#2240 = DIRECTION ( 'NONE',  ( 0.000000000000000000, -0.8090169943749531134, 0.5877852522924653655 ) ) ;
#2241 = DIRECTION ( 'NONE',  ( 0.000000000000000000, 0.000000000000000000, 1.000000000000000000 ) ) ;
#2242 = LINE ( 'NONE', #3971, #1531 ) ;
#2243 = VERTEX_POINT ( 'NONE', #8204 ) ;
#2244 = VERTEX_POINT ( 'NONE', #12574 ) ;
#2245 = CYLINDRICAL_SURFACE ( 'NONE', #9597, 23.50000000000001066 ) ;
#2246 =( GEOMETRIC_REPRESENTATION_CONTEXT ( 3 ) GLOBAL_UNCERTAINTY_ASSIGNED_CONTEXT ( ( #14139 ) ) GLOBAL_UNIT_ASSIGNED_CONTEXT ( ( #8004, #17231, #15165 ) ) REPRESENTATION_CONTEXT ( 'NONE', 'WORKASPACE' ) );
#2247 = EDGE_CURVE ( 'NONE', #5512, #4486, #16682, .T. ) ;
#2248 = ORIENTED_EDGE ( 'NONE', *, *, #341, .F. ) ;
#2249 = DIRECTION ( 'NONE',  ( -1.000000000000000000, -0.000000000000000000, 0.000000000000000000 ) ) ;
#2250 = ADVANCED_FACE ( 'NONE', ( #5897 ), #8844, .T. ) ;
#2251 = DIRECTION ( 'NONE',  ( -1.000000000000000000, 0.000000000000000000, 0.000000000000000000 ) ) ;
#2252 = EDGE_CURVE ( 'NONE', #1940, #1723, #3606, .T. ) ;
#2253 = CYLINDRICAL_SURFACE ( 'NONE', #7817, 2.649999999999999467 ) ;
#2254 = ORIENTED_EDGE ( 'NONE', *, *, #10755, .T. ) ;
#2255 =( GEOMETRIC_REPRESENTATION_CONTEXT ( 3 ) GLOBAL_UNCERTAINTY_ASSIGNED_CONTEXT ( ( #14163 ) ) GLOBAL_UNIT_ASSIGNED_CONTEXT ( ( #3316, #643, #17774 ) ) REPRESENTATION_CONTEXT ( 'NONE', 'WORKASPACE' ) );
#2256 = ORIENTED_EDGE ( 'NONE', *, *, #615, .F. ) ;
#2257 = CARTESIAN_POINT ( 'NONE',  ( 2.742827927723449299, 3.035229711104609596, -3.433252694550591233 ) ) ;
#2258 = CARTESIAN_POINT ( 'NONE',  ( -90.00000000009001155, -34.99999999999999289, -1.301042606982603940E-15 ) ) ;
#2259 = CARTESIAN_POINT ( 'NONE',  ( 34.99999999999999289, 2.055000000000000160, 0.000000000000000000 ) ) ;
#2260 = VERTEX_POINT ( 'NONE', #16093 ) ;
#2261 = DIRECTION ( 'NONE',  ( 0.000000000000000000, 0.000000000000000000, -1.000000000000000000 ) ) ;
#2263 = VERTEX_POINT ( 'NONE', #4293 ) ;
#2262 = EDGE_CURVE ( 'NONE', #16693, #9892, #11198, .T. ) ;
#2264 = DIRECTION ( 'NONE',  ( 0.000000000000000000, 0.000000000000000000, 1.000000000000000000 ) ) ;
#2265 = DIRECTION ( 'NONE',  ( 0.000000000000000000, 0.000000000000000000, 1.000000000000000000 ) ) ;
#2266 = ORIENTED_EDGE ( 'NONE', *, *, #2115, .F. ) ;
#2267 = VERTEX_POINT ( 'NONE', #14659 ) ;
#2268 = FACE_OUTER_BOUND ( 'NONE', #7540, .T. ) ;
#2269 = VERTEX_POINT ( 'NONE', #4471 ) ;
#2270 = DIRECTION ( 'NONE',  ( 0.000000000000000000, 0.000000000000000000, 1.000000000000000000 ) ) ;
#2271 = LINE ( 'NONE', #15705, #10103 ) ;
#2272 = EDGE_CURVE ( 'NONE', #3285, #14075, #11425, .T. ) ;
#2273 = AXIS2_PLACEMENT_3D ( 'NONE', #18038, #9091, #713 ) ;
#2274 = CIRCLE ( 'NONE', #3803, 2.649999999999999467 ) ;
#2275 = ORIENTED_EDGE ( 'NONE', *, *, #14138, .T. ) ;
#2276 = ORIENTED_EDGE ( 'NONE', *, *, #2354, .F. ) ;
#2277 = DIRECTION ( 'NONE',  ( 0.000000000000000000, 0.000000000000000000, 1.000000000000000000 ) ) ;
#2278 = CARTESIAN_POINT ( 'NONE',  ( 4.204115023516791005, -1.660442669500199919, -3.602151381774560068 ) ) ;
#2279 = LINE ( 'NONE', #6675, #17552 ) ;
#2280 = DIRECTION ( 'NONE',  ( -1.000000000000000000, -0.000000000000000000, -0.000000000000000000 ) ) ;
#2281 = EDGE_CURVE ( 'NONE', #1501, #12720, #5292, .T. ) ;
#2282 = CARTESIAN_POINT ( 'NONE',  ( 2.500000000000000000, 2.357898499370432166, -2.385244779468109755E-15 ) ) ;
#2283 = CARTESIAN_POINT ( 'NONE',  ( 0.000000000000000000, -1.178949249685213863, 2.042000000000001148 ) ) ;
#2284 = EDGE_LOOP ( 'NONE', ( #2056, #14725, #15450, #18594 ) ) ;
#2285 = PLANE ( 'NONE',  #14290 ) ;
#2286 = AXIS2_PLACEMENT_3D ( 'NONE', #511, #4890, #905 ) ;
#2287 = LINE ( 'NONE', #15337, #3908 ) ;
#2288 = DIRECTION ( 'NONE',  ( -1.000000000000000000, 0.000000000000000000, 0.000000000000000000 ) ) ;
#2289 = EDGE_CURVE ( 'NONE', #10632, #8217, #5434, .T. ) ;
#2290 = CONTEXT_DEPENDENT_SHAPE_REPRESENTATION ( #8777, #10729 ) ;
#2291 = EDGE_LOOP ( 'NONE', ( #6867, #1141, #4399, #17646 ) ) ;
#2292 = EDGE_LOOP ( 'NONE', ( #6465, #3265, #17753, #3454 ) ) ;
#2293 = EDGE_LOOP ( 'NONE', ( #2111, #1500, #15355, #2594 ) ) ;
#2294 = VECTOR ( 'NONE', #10245, 1000.000000000000000 ) ;
#2295 = CIRCLE ( 'NONE', #787, 0.5155456020628804703 ) ;
#2296 = ORIENTED_EDGE ( 'NONE', *, *, #4987, .T. ) ;
#2297 = CARTESIAN_POINT ( 'NONE',  ( 10.00000000000000000, 19.44239304137403579, -20.41355805489595454 ) ) ;
#2298 = CARTESIAN_POINT ( 'NONE',  ( 10.00000000000000000, -24.68609584167124282, -50.69000562871667626 ) ) ;
#2299 = CARTESIAN_POINT ( 'NONE',  ( -26.29305231718568336, -30.00000000000000000, -16.45302069950552237 ) ) ;
#2300 = CARTESIAN_POINT ( 'NONE',  ( 0.000000000000000000, 46.20417134726178432, -32.31183295104722220 ) ) ;
#2301 = FACE_OUTER_BOUND ( 'NONE', #5097, .T. ) ;
#2302 = EDGE_CURVE ( 'NONE', #7010, #7125, #16069, .T. ) ;
#2303 = DIRECTION ( 'NONE',  ( 0.9995004958639130965, 0.000000000000000000, 0.03160314490350068367 ) ) ;
#2304 = CARTESIAN_POINT ( 'NONE',  ( 5.000000000000000000, 32.46095361140693569, 5.940243314904328109 ) ) ;
#2305 = AXIS2_PLACEMENT_3D ( 'NONE', #6729, #2159, #14151 ) ;
#2306 = DIRECTION ( 'NONE',  ( 0.000000000000000000, -1.000000000000000000, 0.000000000000000000 ) ) ;
#2307 = EDGE_LOOP ( 'NONE', ( #14097, #884, #7375, #8235 ) ) ;
#2308 = CARTESIAN_POINT ( 'NONE',  ( -26.29305231718568336, -30.00000000000000000, -16.45302069950552237 ) ) ;
#2309 = CIRCLE ( 'NONE', #15392, 63.00000000006298961 ) ;
#2310 = ORIENTED_EDGE ( 'NONE', *, *, #9236, .T. ) ;
#2311 = EDGE_CURVE ( 'NONE', #15970, #353, #18501, .T. ) ;
#2312 = AXIS2_PLACEMENT_3D ( 'NONE', #2026, #16502, #15180 ) ;
#2313 = DIRECTION ( 'NONE',  ( 0.000000000000000000, 0.5877852522924685852, 0.8090169943749505599 ) ) ;
#2314 = DIRECTION ( 'NONE',  ( -1.000000000000000000, 0.000000000000000000, 0.000000000000000000 ) ) ;
#2315 = ORIENTED_EDGE ( 'NONE', *, *, #13326, .F. ) ;
#2316 = ORIENTED_EDGE ( 'NONE', *, *, #12234, .F. ) ;
#2317 = AXIS2_PLACEMENT_3D ( 'NONE', #8342, #2901, #10050 ) ;
#2318 = VECTOR ( 'NONE', #1804, 1000.000000000000000 ) ;
#2319 = CARTESIAN_POINT ( 'NONE',  ( 2.500000000000000000, 1.768423874527822459, -1.021000000000002794 ) ) ;
#2320 = DIRECTION ( 'NONE',  ( 1.000000000000000000, 6.123233995736766036E-17, -6.123233995736764803E-17 ) ) ;
#2321 = CARTESIAN_POINT ( 'NONE',  ( 2.595115354961440524, -7.673029147243177306, -1.000000000000000000 ) ) ;
#2322 = EDGE_LOOP ( 'NONE', ( #1922, #4258, #16781, #7012 ) ) ;
#2323 = AXIS2_PLACEMENT_3D ( 'NONE', #16802, #12515, #8135 ) ;
#2324 = CIRCLE ( 'NONE', #7192, 0.7500000000000000000 ) ;
#2325 = CYLINDRICAL_SURFACE ( 'NONE', #16306, 26.24900000002624978 ) ;
#2326 = CARTESIAN_POINT ( 'NONE',  ( -0.3865131578947368918, -23.49682122285426189, -2.000000000000000000 ) ) ;
#2327 = AXIS2_PLACEMENT_3D ( 'NONE', #9831, #10021, #5550 ) ;
#2328 = VECTOR ( 'NONE', #9719, 1000.000000000000000 ) ;
#2329 = CARTESIAN_POINT ( 'NONE',  ( 0.000000000000000000, 32.11449294037196722, 54.20017844242522642 ) ) ;
#2330 = DIRECTION ( 'NONE',  ( -1.000000000000000000, 0.000000000000000000, 0.000000000000000000 ) ) ;
#2331 = VERTEX_POINT ( 'NONE', #8482 ) ;
#2332 = FACE_OUTER_BOUND ( 'NONE', #8917, .T. ) ;
#2333 = ORIENTED_EDGE ( 'NONE', *, *, #13301, .F. ) ;
#2334 = DIRECTION ( 'NONE',  ( 0.000000000000000000, 0.000000000000000000, 1.000000000000000000 ) ) ;
#2335 = DIRECTION ( 'NONE',  ( -1.000000000000000000, -0.000000000000000000, -0.000000000000000000 ) ) ;
#2336 = DIRECTION ( 'NONE',  ( -1.000000000000000000, -0.000000000000000000, -0.000000000000000000 ) ) ;
#2337 = VECTOR ( 'NONE', #5230, 1000.000000000000000 ) ;
#2338 = ORIENTED_EDGE ( 'NONE', *, *, #11370, .F. ) ;
#2339 = EDGE_LOOP ( 'NONE', ( #17775, #17142 ) ) ;
#2340 = DIRECTION ( 'NONE',  ( -1.000000000000000000, -0.000000000000000000, 0.000000000000000000 ) ) ;
#2341 = CONICAL_SURFACE ( 'NONE', #5085, 2.059999999999998721, 0.9599310885968738161 ) ;
#2342 = ORIENTED_EDGE ( 'NONE', *, *, #6563, .T. ) ;
#2343 = CARTESIAN_POINT ( 'NONE',  ( 10.00000000000000000, -49.49802920186203892, -26.71881558261783951 ) ) ;
#2344 = VECTOR ( 'NONE', #9583, 1000.000000000000000 ) ;
#2345 = AXIS2_PLACEMENT_3D ( 'NONE', #6456, #16546, #15131 ) ;
#2346 = EDGE_CURVE ( 'NONE', #806, #2539, #15905, .T. ) ;
#2347 = CARTESIAN_POINT ( 'NONE',  ( 5.000000000000000000, -23.88582760061464327, -22.76987570971553865 ) ) ;
#2348 = EDGE_CURVE ( 'NONE', #912, #13113, #1179, .T. ) ;
#2349 = CIRCLE ( 'NONE', #17867, 33.00000000003299760 ) ;
#2350 = CARTESIAN_POINT ( 'NONE',  ( -11.15000000000000391, 0.000000000000000000, 29.90000000000000213 ) ) ;
#2351 = VERTEX_POINT ( 'NONE', #1253 ) ;
#2352 = PRESENTATION_STYLE_ASSIGNMENT (( #14961 ) ) ;
#2353 = CIRCLE ( 'NONE', #18786, 2.041999999999999815 ) ;
#2354 = EDGE_CURVE ( 'NONE', #16064, #6188, #12953, .T. ) ;
#2355 = ORIENTED_EDGE ( 'NONE', *, *, #7952, .F. ) ;
#2356 = CARTESIAN_POINT ( 'NONE',  ( 10.00000000000000000, 24.79895094899259789, 13.40641754777674421 ) ) ;
#2357 = DIRECTION ( 'NONE',  ( -1.000000000000000000, 0.000000000000000000, 0.000000000000000000 ) ) ;
#2358 = CARTESIAN_POINT ( 'NONE',  ( 0.000000000000000000, 0.000000000000000000, -1.000000000000000000 ) ) ;
#2359 = VERTEX_POINT ( 'NONE', #5987 ) ;
#2360 = DIRECTION ( 'NONE',  ( 0.000000000000000000, 0.000000000000000000, -1.000000000000000000 ) ) ;
#2361 = ORIENTED_EDGE ( 'NONE', *, *, #4802, .T. ) ;
#2362 = EDGE_CURVE ( 'NONE', #18341, #1279, #6951, .T. ) ;
#2363 = CARTESIAN_POINT ( 'NONE',  ( 10.00000000000000000, -24.79895094899250196, -13.40641754777691830 ) ) ;
#2364 = CARTESIAN_POINT ( 'NONE',  ( -10.00000000000000000, 0.000000000000000000, 0.000000000000000000 ) ) ;
#2365 = VERTEX_POINT ( 'NONE', #15722 ) ;
#2366 = EDGE_LOOP ( 'NONE', ( #12175, #4324, #13360, #6401, #3599, #1830, #4859, #11381, #5917, #10798, #7889, #14435, #6870, #2195, #13992, #9394, #7391, #6133, #13256, #3028, #4553, #977, #4853, #12155, #6493, #15310, #6244, #3793, #10062, #8027, #11526, #861, #9036, #5903, #10490, #3546, #12485, #7005, #6649, #1356, #4678, #18808, #11387, #1022, #3314, #8938, #15341, #1113, #11429, #783, #15113, #10313, #4580, #16055, #16529, #1849, #12936, #8649, #13650, #17406, #11669, #14738, #11637, #587, #4304, #14830, #6857, #9441, #18558, #5880, #11416, #5307, #7292, #12744, #13892, #13587, #11400, #10452, #9403, #17096, #6139, #18431, #4031, #9466, #7416 ) ) ;
#2368 = ADVANCED_FACE ( 'NONE', ( #17346 ), #7048, .T. ) ;
#2367 = VERTEX_POINT ( 'NONE', #2672 ) ;
#2369 = LINE ( 'NONE', #13715, #17925 ) ;
#2370 = CYLINDRICAL_SURFACE ( 'NONE', #11303, 56.24900000005625600 ) ;
#2371 = AXIS2_PLACEMENT_3D ( 'NONE', #13985, #17044, #2171 ) ;
#2372 = AXIS2_PLACEMENT_3D ( 'NONE', #11920, #16407, #17729 ) ;
#2373 = VECTOR ( 'NONE', #5928, 1000.000000000000000 ) ;
#2374 = EDGE_CURVE ( 'NONE', #4026, #9705, #10003, .T. ) ;
#2375 = EDGE_CURVE ( 'NONE', #7022, #8500, #17317, .T. ) ;
#2376 = ORIENTED_EDGE ( 'NONE', *, *, #9442, .T. ) ;
#2377 = EDGE_CURVE ( 'NONE', #10560, #1162, #573, .T. ) ;
#2378 = AXIS2_PLACEMENT_3D ( 'NONE', #12154, #3304, #1954 ) ;
#2379 = ORIENTED_EDGE ( 'NONE', *, *, #1440, .T. ) ;
#2380 = DIRECTION ( 'NONE',  ( -1.000000000000000000, 0.000000000000000000, 0.000000000000000000 ) ) ;
#2381 = CARTESIAN_POINT ( 'NONE',  ( 10.00000000000000000, -27.94286728106395756, 3.730438010304225394 ) ) ;
#2383 = EDGE_CURVE ( 'NONE', #16587, #9667, #17428, .T. ) ;
#2382 = CARTESIAN_POINT ( 'NONE',  ( 10.00000000000000000, 9.823366686501460165, -55.51919907100641893 ) ) ;
#2384 = CARTESIAN_POINT ( 'NONE',  ( -4.000000000000000000, 2.511478553582031203, -3.469254451724764543 ) ) ;
#2385 = AXIS2_PLACEMENT_3D ( 'NONE', #12802, #1551, #7265 ) ;
#2386 = SHAPE_REPRESENTATION ( 'circlip for shafts normal_din_Circlip DIN 471 - 50 x 2', ( #8017 ), #3170 ) ;
#2387 = DIRECTION ( 'NONE',  ( 0.000000000000000000, 0.000000000000000000, 1.000000000000000000 ) ) ;
#2388 = FACE_OUTER_BOUND ( 'NONE', #13778, .T. ) ;
#2389 = AXIS2_PLACEMENT_3D ( 'NONE', #16989, #13741, #695 ) ;
#2390 = DIRECTION ( 'NONE',  ( 0.000000000000000000, 0.000000000000000000, 1.000000000000000000 ) ) ;
#2391 = ORIENTED_EDGE ( 'NONE', *, *, #50, .T. ) ;
#2392 = CIRCLE ( 'NONE', #12005, 12.00000000001200817 ) ;
#2393 = DIRECTION ( 'NONE',  ( 0.000000000000000000, 0.000000000000000000, -1.000000000000000000 ) ) ;
#2394 = DIRECTION ( 'NONE',  ( -1.000000000000000000, -0.000000000000000000, 0.000000000000000000 ) ) ;
#2395 = CARTESIAN_POINT ( 'NONE',  ( 2.500000000000000000, -1.178949249685213863, 2.042000000000001148 ) ) ;
#2396 = EDGE_LOOP ( 'NONE', ( #4118, #12826, #1017, #6367 ) ) ;
#2397 = ITEM_DEFINED_TRANSFORMATION ( 'NONE', 'NONE', #2603,  #8017 ) ;
#2398 = EDGE_LOOP ( 'NONE', ( #3586, #10804, #12630, #2943 ) ) ;
#2399 = CIRCLE ( 'NONE', #12429, 0.7499999999999997780 ) ;
#2400 = VECTOR ( 'NONE', #17902, 1000.000000000000000 ) ;
#2401 = ORIENTED_EDGE ( 'NONE', *, *, #12383, .T. ) ;
#2402 = AXIS2_PLACEMENT_3D ( 'NONE', #8200, #11134, #9718 ) ;
#2403 = AXIS2_PLACEMENT_3D ( 'NONE', #1235, #80, #14441 ) ;
#2404 = EDGE_LOOP ( 'NONE', ( #3864, #2415 ) ) ;
#2405 = CARTESIAN_POINT ( 'NONE',  ( 3.309651814758565180, -5.455921364805393026, 0.000000000000000000 ) ) ;
#2406 = DIRECTION ( 'NONE',  ( -1.000000000000000000, 0.000000000000000000, -0.000000000000000000 ) ) ;
#2407 = FILL_AREA_STYLE_COLOUR ( '', #6645 ) ;
#2408 = EDGE_CURVE ( 'NONE', #13973, #9267, #18211, .T. ) ;
#2409 = DIRECTION ( 'NONE',  ( -1.000000000000000000, -0.000000000000000000, -0.000000000000000000 ) ) ;
#2410 = DIRECTION ( 'NONE',  ( 0.000000000000000000, 0.000000000000000000, 1.000000000000000000 ) ) ;
#2411 = DIRECTION ( 'NONE',  ( 0.000000000000000000, 0.000000000000000000, -1.000000000000000000 ) ) ;
#2412 = AXIS2_PLACEMENT_3D ( 'NONE', #9241, #7813, #6485 ) ;
#2413 = CARTESIAN_POINT ( 'NONE',  ( 10.00000000000000000, -62.87238730325622527, 4.007856633823161374 ) ) ;
#2414 = CARTESIAN_POINT ( 'NONE',  ( 10.00000000000000000, -9.514709542736730086, -24.46385708179992946 ) ) ;
#2415 = ORIENTED_EDGE ( 'NONE', *, *, #303, .F. ) ;
#2416 = CARTESIAN_POINT ( 'NONE',  ( 0.000000000000000000, -26.20671763660627462, -1.489278925039791535 ) ) ;
#2417 = ORIENTED_EDGE ( 'NONE', *, *, #11097, .F. ) ;
#2418 = VECTOR ( 'NONE', #7496, 1000.000000000000000 ) ;
#2419 = LINE ( 'NONE', #9458, #14102 ) ;
#2420 = CARTESIAN_POINT ( 'NONE',  ( 2.500000000000000000, 2.357898499370431722, -2.818925648462311528E-15 ) ) ;
#2421 = ORIENTED_EDGE ( 'NONE', *, *, #2141, .T. ) ;
#2422 = VERTEX_POINT ( 'NONE', #17894 ) ;
#2423 = CARTESIAN_POINT ( 'NONE',  ( -3.679171394226034675, -2.494631558665844739, -0.3503314178412558211 ) ) ;
#2424 = DIRECTION ( 'NONE',  ( 1.000000000000000000, 6.123233995736766036E-17, -6.123233995736764803E-17 ) ) ;
#2425 = CARTESIAN_POINT ( 'NONE',  ( 0.000000000000000000, 5.940243314904213534, 32.46095361140695701 ) ) ;
#2426 = ORIENTED_EDGE ( 'NONE', *, *, #14464, .T. ) ;
#2427 = CIRCLE ( 'NONE', #7884, 56.24900000005625600 ) ;
#2428 = AXIS2_PLACEMENT_3D ( 'NONE', #9490, #9201, #9399 ) ;
#2429 = CARTESIAN_POINT ( 'NONE',  ( 0.000000000000000000, 0.000000000000000000, 0.000000000000000000 ) ) ;
#2430 = LINE ( 'NONE', #12905, #8813 ) ;
#2431 = CARTESIAN_POINT ( 'NONE',  ( -90.00000000009001155, -38.00000000000000000, -1.301042606982603940E-15 ) ) ;
#2432 = EDGE_CURVE ( 'NONE', #1905, #16921, #7302, .T. ) ;
#2433 = CYLINDRICAL_SURFACE ( 'NONE', #18608, 0.7499999999999997780 ) ;
#2434 = EDGE_LOOP ( 'NONE', ( #16013, #12350, #1725, #15793 ) ) ;
#2435 = CYLINDRICAL_SURFACE ( 'NONE', #8768, 5.000000000000004441 ) ;
#2436 = ORIENTED_EDGE ( 'NONE', *, *, #1360, .F. ) ;
#2437 = CARTESIAN_POINT ( 'NONE',  ( 10.00000000000000000, 33.95787273855309252, -45.00825343884985585 ) ) ;
#2438 = DIRECTION ( 'NONE',  ( -1.000000000000000000, 0.000000000000000000, 0.000000000000000000 ) ) ;
#2440 = DIRECTION ( 'NONE',  ( -1.000000000000000000, 0.000000000000000000, 0.000000000000000000 ) ) ;
#2439 = VECTOR ( 'NONE', #7371, 1000.000000000000000 ) ;
#2441 = EDGE_LOOP ( 'NONE', ( #2463, #5836, #1638, #3081 ) ) ;
#2442 = ORIENTED_EDGE ( 'NONE', *, *, #12289, .F. ) ;
#2443 = CARTESIAN_POINT ( 'NONE',  ( 3.367778697655221307E-15, -13.75000000000000355, -27.50000000000000000 ) ) ;
#2444 = ORIENTED_EDGE ( 'NONE', *, *, #7325, .F. ) ;
#2445 = CARTESIAN_POINT ( 'NONE',  ( 2.500000000000000000, 0.000000000000000000, 0.000000000000000000 ) ) ;
#2446 = ADVANCED_FACE ( 'NONE', ( #13709 ), #4848, .T. ) ;
#2447 = EDGE_CURVE ( 'NONE', #4207, #9803, #7569, .T. ) ;
#2448 = DIRECTION ( 'NONE',  ( 0.000000000000000000, 0.000000000000000000, 1.000000000000000000 ) ) ;
#2449 = CYLINDRICAL_SURFACE ( 'NONE', #2033, 4.799999999999998934 ) ;
#2450 = ORIENTED_EDGE ( 'NONE', *, *, #17509, .F. ) ;
#2451 = CARTESIAN_POINT ( 'NONE',  ( 0.000000000000000000, 0.000000000000000000, 0.000000000000000000 ) ) ;
#2452 = AXIS2_PLACEMENT_3D ( 'NONE', #15849, #11469, #1090 ) ;
#2453 = ORIENTED_EDGE ( 'NONE', *, *, #6974, .T. ) ;
#2454 = DIRECTION ( 'NONE',  ( -1.000000000000000000, -0.000000000000000000, -0.000000000000000000 ) ) ;
#2455 = DIRECTION ( 'NONE',  ( 0.000000000000000000, 0.000000000000000000, 1.000000000000000000 ) ) ;
#2456 = FACE_OUTER_BOUND ( 'NONE', #335, .T. ) ;
#2457 = ORIENTED_EDGE ( 'NONE', *, *, #15300, .F. ) ;
#2458 = DIRECTION ( 'NONE',  ( -0.000000000000000000, -0.000000000000000000, -1.000000000000000000 ) ) ;
#2459 = EDGE_LOOP ( 'NONE', ( #8753, #6365, #5072, #5009 ) ) ;
#2460 = CARTESIAN_POINT ( 'NONE',  ( -85.22968676783801811, 1.821459649775647449E-14, -0.5330212624288650503 ) ) ;
#2461 = DIRECTION ( 'NONE',  ( 0.000000000000000000, 0.000000000000000000, 1.000000000000000000 ) ) ;
#2462 = ORIENTED_EDGE ( 'NONE', *, *, #9683, .T. ) ;
#2463 = ORIENTED_EDGE ( 'NONE', *, *, #14012, .F. ) ;
#2464 = FACE_OUTER_BOUND ( 'NONE', #12003, .T. ) ;
#2465 = ADVANCED_FACE ( 'NONE', ( #284 ), #10653, .T. ) ;
#2466 = ORIENTED_EDGE ( 'NONE', *, *, #4485, .T. ) ;
#2467 = CARTESIAN_POINT ( 'NONE',  ( 5.032868406504333869, -28.36021363089093938, -2.000000000000000000 ) ) ;
#2468 = DIRECTION ( 'NONE',  ( -1.000000000000000000, 0.000000000000000000, 0.000000000000000000 ) ) ;
#2469 = AXIS2_PLACEMENT_3D ( 'NONE', #16287, #3786, #3247 ) ;
#2470 = VERTEX_POINT ( 'NONE', #15035 ) ;
#2471 = VERTEX_POINT ( 'NONE', #8932 ) ;
#2472 = DIRECTION ( 'NONE',  ( -1.000000000000000000, -0.000000000000000000, -0.000000000000000000 ) ) ;
#2473 = CARTESIAN_POINT ( 'NONE',  ( 4.197310751797292738, 0.8178363989516252985, -3.502498386812444409 ) ) ;
#2474 = DIRECTION ( 'NONE',  ( 0.000000000000000000, -0.3090169943749547787, 0.9510565162951511997 ) ) ;
#2475 = DIRECTION ( 'NONE',  ( 1.000000000000000000, 0.000000000000000000, 0.000000000000000000 ) ) ;
#2476 = AXIS2_PLACEMENT_3D ( 'NONE', #10047, #7175, #17298 ) ;
#2477 = CARTESIAN_POINT ( 'NONE',  ( 10.00000000000000000, -55.51919907100660367, 9.823366686500467182 ) ) ;
#2478 = LINE ( 'NONE', #8295, #2192 ) ;
#2479 = CARTESIAN_POINT ( 'NONE',  ( 2.500000000000000000, -1.178949249685213863, 2.042000000000001148 ) ) ;
#2480 = ORIENTED_EDGE ( 'NONE', *, *, #10652, .T. ) ;
#2481 = DIRECTION ( 'NONE',  ( -1.000000000000000000, 0.000000000000000000, 0.000000000000000000 ) ) ;
#2482 = EDGE_CURVE ( 'NONE', #13703, #17590, #4239, .T. ) ;
#2483 = EDGE_CURVE ( 'NONE', #4644, #1826, #6669, .T. ) ;
#2484 = DIRECTION ( 'NONE',  ( -1.000000000000000000, 0.000000000000000000, 0.000000000000000000 ) ) ;
#2485 = CIRCLE ( 'NONE', #15568, 30.39999999999999858 ) ;
#2486 = EDGE_CURVE ( 'NONE', #1187, #11652, #1789, .T. ) ;
#2487 = DIRECTION ( 'NONE',  ( 0.03086419753086420623, 0.9995235871707959241, -0.000000000000000000 ) ) ;
#2488 = DIRECTION ( 'NONE',  ( 0.000000000000000000, 0.000000000000000000, -1.000000000000000000 ) ) ;
#2489 = EDGE_CURVE ( 'NONE', #17607, #15207, #2392, .T. ) ;
#2490 = VERTEX_POINT ( 'NONE', #16271 ) ;
#2491 = EDGE_CURVE ( 'NONE', #17597, #2625, #3627, .T. ) ;
#2492 = ORIENTED_EDGE ( 'NONE', *, *, #4160, .T. ) ;
#2493 = ORIENTED_EDGE ( 'NONE', *, *, #8105, .F. ) ;
#2494 = ADVANCED_FACE ( 'NONE', ( #11888 ), #13334, .F. ) ;
#2496 = DIRECTION ( 'NONE',  ( 1.000000000000000000, 0.000000000000000000, 0.000000000000000000 ) ) ;
#2495 = AXIS2_PLACEMENT_3D ( 'NONE', #8563, #89, #1329 ) ;
#2497 = CARTESIAN_POINT ( 'NONE',  ( -290.0000000000001137, -30.00000000000000000, -125.0000000000000000 ) ) ;
#2498 = SURFACE_SIDE_STYLE ('',( #9739 ) ) ;
#2499 = CYLINDRICAL_SURFACE ( 'NONE', #10518, 2.649999999999995914 ) ;
#2500 = DIRECTION ( 'NONE',  ( 0.000000000000000000, -1.000000000000000000, 0.000000000000000000 ) ) ;
#2501 = DIRECTION ( 'NONE',  ( -0.000000000000000000, 1.000000000000000000, -0.000000000000000000 ) ) ;
#2502 = DIRECTION ( 'NONE',  ( 0.000000000000000000, -0.7071067811865389130, -0.7071067811865561215 ) ) ;
#2503 = CARTESIAN_POINT ( 'NONE',  ( 0.000000000000000000, 44.70888270294162226, 34.13306034420202906 ) ) ;
#2504 = ORIENTED_EDGE ( 'NONE', *, *, #17397, .T. ) ;
#2505 = DIRECTION ( 'NONE',  ( 1.000000000000000000, 0.000000000000000000, 0.000000000000000000 ) ) ;
#2506 = ORIENTED_EDGE ( 'NONE', *, *, #619, .F. ) ;
#2507 = EDGE_CURVE ( 'NONE', #10912, #16587, #3013, .T. ) ;
#2508 = DIRECTION ( 'NONE',  ( -1.000000000000000000, -0.000000000000000000, -0.000000000000000000 ) ) ;
#2509 = DIRECTION ( 'NONE',  ( 0.000000000000000000, 0.3090169943749411785, 0.9510565162951556406 ) ) ;
#2510 = ORIENTED_EDGE ( 'NONE', *, *, #1946, .T. ) ;
#2511 = CYLINDRICAL_SURFACE ( 'NONE', #17239, 24.00000000002399858 ) ;
#2512 = CARTESIAN_POINT ( 'NONE',  ( 32.50000000000000000, -39.99999999999999289, 3.642919299551294898E-13 ) ) ;
#2513 = AXIS2_PLACEMENT_3D ( 'NONE', #6551, #12358, #5124 ) ;
#2514 = CARTESIAN_POINT ( 'NONE',  ( -26.29305231718584324, -34.99999999999999289, 16.45302069950530566 ) ) ;
#2515 = VERTEX_POINT ( 'NONE', #9308 ) ;
#2516 = ADVANCED_FACE ( 'NONE', ( #15138 ), #1802, .T. ) ;
#2517 = SHAPE_REPRESENTATION ( 'hex flange nut gradea_iso_ISO - 4161 - M5 - N', ( #8017 ), #6229 ) ;
#2518 = LINE ( 'NONE', #719, #14481 ) ;
#2519 = CARTESIAN_POINT ( 'NONE',  ( 10.00000000000000000, 0.000000000000000000, 0.000000000000000000 ) ) ;
#2520 = CARTESIAN_POINT ( 'NONE',  ( 10.00000000000000000, -50.69000562871624993, -24.68609584167212745 ) ) ;
#2521 = CARTESIAN_POINT ( 'NONE',  ( 0.000000000000000000, -5.940243314904443572, 32.46095361140691438 ) ) ;
#2522 = AXIS2_PLACEMENT_3D ( 'NONE', #3970, #14145, #14249 ) ;
#2523 = CIRCLE ( 'NONE', #17715, 63.00000000006298961 ) ;
#2524 = VECTOR ( 'NONE', #2288, 1000.000000000000000 ) ;
#2525 = DIRECTION ( 'NONE',  ( 0.000000000000000000, 0.000000000000000000, 1.000000000000000000 ) ) ;
#2526 = ORIENTED_EDGE ( 'NONE', *, *, #13067, .T. ) ;
#2527 = CARTESIAN_POINT ( 'NONE',  ( 10.00000000000000000, 0.000000000000000000, 0.000000000000000000 ) ) ;
#2528 = DIRECTION ( 'NONE',  ( 1.000000000000000000, 0.000000000000000000, 0.000000000000000000 ) ) ;
#2529 = CARTESIAN_POINT ( 'NONE',  ( 0.000000000000000000, -27.94286728106395756, 3.730438010304225394 ) ) ;
#2530 = VERTEX_POINT ( 'NONE', #11978 ) ;
#2531 = VERTEX_POINT ( 'NONE', #17790 ) ;
#2532 = CARTESIAN_POINT ( 'NONE',  ( 10.00000000000000000, -9.514709542736730086, -24.46385708179992946 ) ) ;
#2533 = ORIENTED_EDGE ( 'NONE', *, *, #12490, .F. ) ;
#2534 = DIRECTION ( 'NONE',  ( -0.000000000000000000, 1.000000000000000000, -0.000000000000000000 ) ) ;
#2535 = EDGE_CURVE ( 'NONE', #12076, #1784, #10557, .T. ) ;
#2536 = CIRCLE ( 'NONE', #1621, 12.00000000001200462 ) ;
#2537 = DIRECTION ( 'NONE',  ( 1.000000000000000000, -0.000000000000000000, -0.000000000000000000 ) ) ;
#2538 = CARTESIAN_POINT ( 'NONE',  ( 5.000000000000000000, 62.87238730325621106, 4.007856633823612569 ) ) ;
#2539 = VERTEX_POINT ( 'NONE', #9131 ) ;
#2540 = ORIENTED_EDGE ( 'NONE', *, *, #8625, .F. ) ;
#2542 = FACE_OUTER_BOUND ( 'NONE', #8712, .T. ) ;
#2541 = PRODUCT_DEFINITION_CONTEXT ( 'detailed design', #9758, 'design' ) ;
#2543 = DIRECTION ( 'NONE',  ( -1.000000000000000000, -0.000000000000000000, -0.000000000000000000 ) ) ;
#2544 = DIRECTION ( 'NONE',  ( 0.000000000000000000, 0.000000000000000000, -1.000000000000000000 ) ) ;
#2545 = EDGE_LOOP ( 'NONE', ( #10844, #253, #1321, #75 ) ) ;
#2546 = LINE ( 'NONE', #11220, #15742 ) ;
#2547 = ORIENTED_EDGE ( 'NONE', *, *, #4709, .T. ) ;
#2548 = AXIS2_PLACEMENT_3D ( 'NONE', #18401, #11647, #12898 ) ;
#2549 = EDGE_CURVE ( 'NONE', #8661, #3056, #6044, .T. ) ;
#2550 = CARTESIAN_POINT ( 'NONE',  ( 0.000000000000000000, 0.000000000000000000, 0.000000000000000000 ) ) ;
#2551 = LINE ( 'NONE', #11117, #17123 ) ;
#2552 = ORIENTED_EDGE ( 'NONE', *, *, #14420, .F. ) ;
#2553 = ORIENTED_EDGE ( 'NONE', *, *, #10792, .F. ) ;
#2554 = CARTESIAN_POINT ( 'NONE',  ( 10.00000000000000000, -24.79895094899269026, 13.40641754777657013 ) ) ;
#2555 = EDGE_CURVE ( 'NONE', #12447, #13033, #3324, .T. ) ;
#2556 = ORIENTED_EDGE ( 'NONE', *, *, #13530, .T. ) ;
#2557 = LINE ( 'NONE', #17233, #7575 ) ;
#2558 = DIRECTION ( 'NONE',  ( -1.000000000000000000, -0.000000000000000000, 0.000000000000000000 ) ) ;
#2559 =( GEOMETRIC_REPRESENTATION_CONTEXT ( 3 ) GLOBAL_UNCERTAINTY_ASSIGNED_CONTEXT ( ( #12436 ) ) GLOBAL_UNIT_ASSIGNED_CONTEXT ( ( #5426, #3996, #5518 ) ) REPRESENTATION_CONTEXT ( 'NONE', 'WORKASPACE' ) );
#2560 = ORIENTED_EDGE ( 'NONE', *, *, #6446, .F. ) ;
#2561 = VERTEX_POINT ( 'NONE', #951 ) ;
#2562 = DIRECTION ( 'NONE',  ( 0.000000000000000000, -0.4539904997395542430, 0.8910065241883641241 ) ) ;
#2563 = LINE ( 'NONE', #18758, #1788 ) ;
#2564 = DIRECTION ( 'NONE',  ( -1.000000000000000000, 0.000000000000000000, 0.000000000000000000 ) ) ;
#2565 = CARTESIAN_POINT ( 'NONE',  ( 1.734723475976807094E-15, 4.618802153517012954, -0.4999999999999995559 ) ) ;
#2566 = LINE ( 'NONE', #9722, #15457 ) ;
#2567 = CARTESIAN_POINT ( 'NONE',  ( -11.25000000000000355, 0.000000000000000000, 0.000000000000000000 ) ) ;
#2568 = DIRECTION ( 'NONE',  ( -0.000000000000000000, 1.000000000000000000, -0.000000000000000000 ) ) ;
#2569 = ORIENTED_EDGE ( 'NONE', *, *, #8105, .T. ) ;
#2570 = DIRECTION ( 'NONE',  ( -0.000000000000000000, -1.000000000000000000, -0.000000000000000000 ) ) ;
#2571 = CARTESIAN_POINT ( 'NONE',  ( 10.00000000000000000, 27.94286728106393269, 3.730438010304423013 ) ) ;
#2572 =( GEOMETRIC_REPRESENTATION_CONTEXT ( 3 ) GLOBAL_UNCERTAINTY_ASSIGNED_CONTEXT ( ( #1030 ) ) GLOBAL_UNIT_ASSIGNED_CONTEXT ( ( #12629, #11201, #17028 ) ) REPRESENTATION_CONTEXT ( 'NONE', 'WORKASPACE' ) );
#2573 = LINE ( 'NONE', #2867, #18208 ) ;
#2574 = LINE ( 'NONE', #15729, #1906 ) ;
#2575 = AXIS2_PLACEMENT_3D ( 'NONE', #9026, #13329, #16266 ) ;
#2576 = ITEM_DEFINED_TRANSFORMATION ( 'NONE', 'NONE', #6239,  #8017 ) ;
#2577 = EDGE_LOOP ( 'NONE', ( #2866, #8006, #16344, #3214 ) ) ;
#2578 = ORIENTED_EDGE ( 'NONE', *, *, #11344, .F. ) ;
#2579 = EDGE_CURVE ( 'NONE', #1626, #4084, #16656, .T. ) ;
#2580 = EDGE_LOOP ( 'NONE', ( #4963, #18151 ) ) ;
#2581 =( GEOMETRIC_REPRESENTATION_CONTEXT ( 3 ) GLOBAL_UNCERTAINTY_ASSIGNED_CONTEXT ( ( #10529 ) ) GLOBAL_UNIT_ASSIGNED_CONTEXT ( ( #2225, #18319, #3850 ) ) REPRESENTATION_CONTEXT ( 'NONE', 'WORKASPACE' ) );
#2582 = LINE ( 'NONE', #2690, #16318 ) ;
#2583 = EDGE_CURVE ( 'NONE', #18126, #9305, #8169, .T. ) ;
#2584 = SURFACE_SIDE_STYLE ('',( #9832 ) ) ;
#2585 = CIRCLE ( 'NONE', #4407, 12.00000000001200462 ) ;
#2586 = ORIENTED_EDGE ( 'NONE', *, *, #1555, .T. ) ;
#2587 = SURFACE_STYLE_USAGE ( .BOTH. , #15640 ) ;
#2588 = VECTOR ( 'NONE', #10689, 1000.000000000000000 ) ;
#2589 = CARTESIAN_POINT ( 'NONE',  ( -5.686050877451574337, -5.768780236673276995, 0.000000000000000000 ) ) ;
#2590 = EDGE_CURVE ( 'NONE', #5558, #16747, #12648, .T. ) ;
#2591 = DIRECTION ( 'NONE',  ( 0.000000000000000000, 0.000000000000000000, -1.000000000000000000 ) ) ;
#2592 = CARTESIAN_POINT ( 'NONE',  ( 0.000000000000000000, -30.00000000000000000, 0.000000000000000000 ) ) ;
#2593 = CARTESIAN_POINT ( 'NONE',  ( 32.50000000000000000, -34.99999999999999289, 3.680389326632394941E-13 ) ) ;
#2594 = ORIENTED_EDGE ( 'NONE', *, *, #18748, .T. ) ;
#2595 = DIRECTION ( 'NONE',  ( 0.000000000000000000, 0.000000000000000000, 1.000000000000000000 ) ) ;
#2596 = ORIENTED_EDGE ( 'NONE', *, *, #16589, .T. ) ;
#2597 = EDGE_CURVE ( 'NONE', #9337, #10165, #1487, .T. ) ;
#2598 = LINE ( 'NONE', #2991, #542 ) ;
#2599 = VERTEX_POINT ( 'NONE', #14171 ) ;
#2600 = AXIS2_PLACEMENT_3D ( 'NONE', #6445, #3402, #3121 ) ;
#2601 = FACE_OUTER_BOUND ( 'NONE', #13429, .T. ) ;
#2602 = CARTESIAN_POINT ( 'NONE',  ( 13.90576474687237152, -14.99999999999999289, 42.79754323328199206 ) ) ;
#2603 = AXIS2_PLACEMENT_3D ( 'NONE', #5566, #11277, #17099 ) ;
#2604 = DIRECTION ( 'NONE',  ( -1.000000000000000000, 0.000000000000000000, 0.000000000000000000 ) ) ;
#2605 = ORIENTED_EDGE ( 'NONE', *, *, #12034, .T. ) ;
#2606 = EDGE_CURVE ( 'NONE', #15209, #1489, #10008, .T. ) ;
#2607 = VECTOR ( 'NONE', #7345, 1000.000000000000000 ) ;
#2608 = EDGE_CURVE ( 'NONE', #923, #17584, #18270, .T. ) ;
#2609 = DIRECTION ( 'NONE',  ( 0.000000000000000000, -0.5000000000000011102, -0.8660254037844379305 ) ) ;
#2610 = EDGE_CURVE ( 'NONE', #5270, #3414, #9698, .T. ) ;
#2611 = FACE_OUTER_BOUND ( 'NONE', #13479, .T. ) ;
#2612 = CIRCLE ( 'NONE', #6253, 2.649999999999999467 ) ;
#2613 = LINE ( 'NONE', #5188, #5408 ) ;
#2614 = CARTESIAN_POINT ( 'NONE',  ( 10.00000000000000000, 0.000000000000000000, 0.000000000000000000 ) ) ;
#2615 = EDGE_CURVE ( 'NONE', #4819, #2625, #15231, .T. ) ;
#2616 = AXIS2_PLACEMENT_3D ( 'NONE', #7357, #11281, #2892 ) ;
#2617 = CARTESIAN_POINT ( 'NONE',  ( 5.000000000000000000, 14.27431201565567243, -29.75305054077457356 ) ) ;
#2618 = CIRCLE ( 'NONE', #15396, 12.00000000001200817 ) ;
#2619 = VERTEX_POINT ( 'NONE', #2174 ) ;
#2620 = EDGE_CURVE ( 'NONE', #12166, #12513, #10304, .T. ) ;
#2621 = DIRECTION ( 'NONE',  ( 0.000000000000000000, 0.000000000000000000, -1.000000000000000000 ) ) ;
#2622 = DIRECTION ( 'NONE',  ( 0.000000000000000000, 0.000000000000000000, 1.000000000000000000 ) ) ;
#2623 = FACE_OUTER_BOUND ( 'NONE', #13642, .T. ) ;
#2624 = EDGE_LOOP ( 'NONE', ( #8240, #18567, #14708, #5265 ) ) ;
#2625 = VERTEX_POINT ( 'NONE', #13990 ) ;
#2626 = DIRECTION ( 'NONE',  ( 0.000000000000000000, 1.000000000000000000, 0.000000000000000000 ) ) ;
#2627 =( NAMED_UNIT ( * ) PLANE_ANGLE_UNIT ( ) SI_UNIT ( $, .RADIAN. ) );
#2628 = EDGE_LOOP ( 'NONE', ( #5943, #3535, #15510, #6181 ) ) ;
#2629 = FACE_OUTER_BOUND ( 'NONE', #18606, .T. ) ;
#2630 = AXIS2_PLACEMENT_3D ( 'NONE', #8418, #2472, #15244 ) ;
#2631 = AXIS2_PLACEMENT_3D ( 'NONE', #7517, #12084, #373 ) ;
#2632 = VECTOR ( 'NONE', #119, 1000.000000000000000 ) ;
#2633 = AXIS2_PLACEMENT_3D ( 'NONE', #6245, #17768, #15017 ) ;
#2634 = DIRECTION ( 'NONE',  ( 0.000000000000000000, 0.9510565162951543083, -0.3090169943749447312 ) ) ;
#2635 = CARTESIAN_POINT ( 'NONE',  ( 2.500000000000000000, 0.000000000000000000, 0.000000000000000000 ) ) ;
#2636 = ORIENTED_EDGE ( 'NONE', *, *, #15650, .T. ) ;
#2637 = DIRECTION ( 'NONE',  ( 0.000000000000000000, 0.000000000000000000, -1.000000000000000000 ) ) ;
#2638 = AXIS2_PLACEMENT_3D ( 'NONE', #14376, #1336, #17512 ) ;
#2639 = ORIENTED_EDGE ( 'NONE', *, *, #16358, .T. ) ;
#2640 = DIRECTION ( 'NONE',  ( -0.000000000000000000, 1.000000000000000000, -0.000000000000000000 ) ) ;
#2641 = CARTESIAN_POINT ( 'NONE',  ( 0.000000000000000000, 0.000000000000000000, 0.000000000000000000 ) ) ;
#2643 = AXIS2_PLACEMENT_3D ( 'NONE', #84, #11515, #18741 ) ;
#2642 = CARTESIAN_POINT ( 'NONE',  ( 2.250000000000000000, -27.60846790388774608, 0.000000000000000000 ) ) ;
#2644 = EDGE_LOOP ( 'NONE', ( #18035, #9393, #17813, #7720 ) ) ;
#2645 = CARTESIAN_POINT ( 'NONE',  ( 10.00000000000000000, -13.79392154159178219, 61.47135697633773788 ) ) ;
#2646 = EDGE_CURVE ( 'NONE', #5108, #478, #9089, .T. ) ;
#2647 = ORIENTED_EDGE ( 'NONE', *, *, #6446, .T. ) ;
#2648 = CIRCLE ( 'NONE', #12683, 2.100000000000000089 ) ;
#2649 = PLANE ( 'NONE',  #7273 ) ;
#2650 = FACE_OUTER_BOUND ( 'NONE', #3807, .T. ) ;
#2651 = VECTOR ( 'NONE', #16286, 1000.000000000000000 ) ;
#2652 = VERTEX_POINT ( 'NONE', #13889 ) ;
#2653 = ORIENTED_EDGE ( 'NONE', *, *, #4000, .F. ) ;
#2654 = VECTOR ( 'NONE', #9756, 1000.000000000000000 ) ;
#2655 = DIRECTION ( 'NONE',  ( -1.000000000000000000, 0.000000000000000000, 0.000000000000000000 ) ) ;
#2656 = ORIENTED_EDGE ( 'NONE', *, *, #10515, .T. ) ;
#2657 = CARTESIAN_POINT ( 'NONE',  ( 10.00000000000000000, 0.000000000000000000, 0.000000000000000000 ) ) ;
#2658 = CARTESIAN_POINT ( 'NONE',  ( 10.00000000000000000, 44.70888270294162226, 34.13306034420202906 ) ) ;
#2659 = CIRCLE ( 'NONE', #15738, 27.29487558977753991 ) ;
#2660 = CIRCLE ( 'NONE', #4482, 24.00000000002399503 ) ;
#2661 = ADVANCED_FACE ( 'NONE', ( #856 ), #5123, .F. ) ;
#2662 = AXIS2_PLACEMENT_3D ( 'NONE', #1007, #9762, #8037 ) ;
#2663 = AXIS2_PLACEMENT_3D ( 'NONE', #5595, #18553, #16228 ) ;
#2664 = ORIENTED_EDGE ( 'NONE', *, *, #3537, .T. ) ;
#2665 = EDGE_CURVE ( 'NONE', #15635, #4270, #10931, .T. ) ;
#2666 = PRODUCT ( 'circlip for shafts normal_din_Circlip DIN 471 - 10 x 1', 'circlip for shafts normal_din_Circlip DIN 471 - 10 x 1', '', ( #221 ) ) ;
#2667 = ORIENTED_EDGE ( 'NONE', *, *, #8550, .F. ) ;
#2668 = CYLINDRICAL_SURFACE ( 'NONE', #2638, 6.080745460913608902 ) ;
#2669 = CARTESIAN_POINT ( 'NONE',  ( -2.804994570502171047, -3.229033611042465335, -3.526374918436838701 ) ) ;
#2670 = DIRECTION ( 'NONE',  ( 1.000000000000000000, 0.000000000000000000, 0.000000000000000000 ) ) ;
#2671 = LINE ( 'NONE', #10001, #13888 ) ;
#2672 = CARTESIAN_POINT ( 'NONE',  ( 2.500000000000000888, 3.061616997868384127E-16, -4.974599999999998801 ) ) ;
#2673 = CARTESIAN_POINT ( 'NONE',  ( 0.000000000000000000, 0.000000000000000000, 0.000000000000000000 ) ) ;
#2674 = AXIS2_PLACEMENT_3D ( 'NONE', #15879, #15794, #7202 ) ;
#2675 = DIRECTION ( 'NONE',  ( 0.000000000000000000, 0.8660254037844380415, -0.5000000000000009992 ) ) ;
#2676 = EDGE_LOOP ( 'NONE', ( #16795, #16322, #14563, #9445, #11509, #13442, #5776, #13951, #6134, #9208, #1287 ) ) ;
#2677 = DIRECTION ( 'NONE',  ( 0.000000000000000000, 0.000000000000000000, 1.000000000000000000 ) ) ;
#2678 = CARTESIAN_POINT ( 'NONE',  ( -90.00000000009001155, -29.99899999999999878, -1.301042606982605321E-15 ) ) ;
#2679 = VECTOR ( 'NONE', #12131, 1000.000000000000000 ) ;
#2680 = DIRECTION ( 'NONE',  ( 0.000000000000000000, 0.000000000000000000, -1.000000000000000000 ) ) ;
#2681 = EDGE_LOOP ( 'NONE', ( #9489, #3434, #9838, #1517 ) ) ;
#2682 = VECTOR ( 'NONE', #17297, 1000.000000000000114 ) ;
#2683 = VECTOR ( 'NONE', #17540, 1000.000000000000000 ) ;
#2684 = ORIENTED_EDGE ( 'NONE', *, *, #13908, .T. ) ;
#2685 = EDGE_CURVE ( 'NONE', #743, #16490, #9595, .T. ) ;
#2686 = AXIS2_PLACEMENT_3D ( 'NONE', #1106, #15379, #3967 ) ;
#2687 = ORIENTED_EDGE ( 'NONE', *, *, #2001, .T. ) ;
#2688 = CIRCLE ( 'NONE', #9668, 26.24900000002625688 ) ;
#2689 = ADVANCED_FACE ( 'NONE', ( #15416 ), #17049, .T. ) ;
#2690 = CARTESIAN_POINT ( 'NONE',  ( 3.061616997868383043E-15, -30.00000000000000000, -25.00000000000000000 ) ) ;
#2691 = CARTESIAN_POINT ( 'NONE',  ( -90.40196296004810961, -10.00000000000001954, 6.951864913735148477 ) ) ;
#2692 = VERTEX_POINT ( 'NONE', #11116 ) ;
#2693 = AXIS2_PLACEMENT_3D ( 'NONE', #13, #1611, #13145 ) ;
#2694 = CARTESIAN_POINT ( 'NONE',  ( -90.00000000009001155, -10.00000000000001776, -1.301042606982605912E-15 ) ) ;
#2695 = DIRECTION ( 'NONE',  ( -0.000000000000000000, 1.000000000000000000, 0.000000000000000000 ) ) ;
#2696 = CARTESIAN_POINT ( 'NONE',  ( -90.00000000009001155, -13.00000000000001776, 5.000000000000003553 ) ) ;
#2697 = CARTESIAN_POINT ( 'NONE',  ( -0.3865131578947368918, -23.49682122285426189, -2.000000000000000000 ) ) ;
#2698 = VERTEX_POINT ( 'NONE', #3897 ) ;
#2699 = CARTESIAN_POINT ( 'NONE',  ( -4.000000000000000000, 0.3987449864459974846, -0.01220643443059782861 ) ) ;
#2700 = ORIENTED_EDGE ( 'NONE', *, *, #6226, .T. ) ;
#2701 = DIRECTION ( 'NONE',  ( 0.000000000000000000, 0.000000000000000000, 1.000000000000000000 ) ) ;
#2702 = AXIS2_PLACEMENT_3D ( 'NONE', #329, #3468, #11936 ) ;
#2703 = VERTEX_POINT ( 'NONE', #2460 ) ;
#2704 = EDGE_CURVE ( 'NONE', #14291, #2833, #9792, .T. ) ;
#2705 = PRODUCT_CONTEXT ( 'NONE', #4283, 'mechanical' ) ;
#2706 = AXIS2_PLACEMENT_3D ( 'NONE', #7616, #13433, #8939 ) ;
#2708 = EDGE_CURVE ( 'NONE', #9496, #8847, #13648, .T. ) ;
#2707 = CARTESIAN_POINT ( 'NONE',  ( 10.00000000000000000, 53.06836994729233936, 18.64666490672390964 ) ) ;
#2709 = VERTEX_POINT ( 'NONE', #8826 ) ;
#2710 = CONICAL_SURFACE ( 'NONE', #16394, 5.560781378645573980, 1.221730476396046816 ) ;
#2711 = VECTOR ( 'NONE', #15694, 1000.000000000000000 ) ;
#2712 = EDGE_CURVE ( 'NONE', #8620, #8889, #1196, .T. ) ;
#2713 = DIRECTION ( 'NONE',  ( 1.000000000000000000, 0.000000000000000000, -0.000000000000000000 ) ) ;
#2714 = DIRECTION ( 'NONE',  ( 0.000000000000000000, 0.000000000000000000, -1.000000000000000000 ) ) ;
#2715 = CIRCLE ( 'NONE', #6973, 2.649999999999995914 ) ;
#2716 = CARTESIAN_POINT ( 'NONE',  ( -6.473970235329672780E-16, -4.862606272033106691, -3.745885042887442395 ) ) ;
#2717 = DIRECTION ( 'NONE',  ( 0.000000000000000000, 0.000000000000000000, 1.000000000000000000 ) ) ;
#2718 = AXIS2_PLACEMENT_3D ( 'NONE', #2844, #15517, #9799 ) ;
#2719 = CARTESIAN_POINT ( 'NONE',  ( -56.50000000009000445, -30.00000000000000000, -2.649999999999610889 ) ) ;
#2720 = ORIENTED_EDGE ( 'NONE', *, *, #14352, .F. ) ;
#2721 = DIRECTION ( 'NONE',  ( -1.000000000000000000, -0.000000000000000000, -0.000000000000000000 ) ) ;
#2722 = CARTESIAN_POINT ( 'NONE',  ( 4.000000000000000000, 2.309401076758497151, -5.000000000000000000 ) ) ;
#2723 = FACE_OUTER_BOUND ( 'NONE', #12700, .T. ) ;
#2724 = VERTEX_POINT ( 'NONE', #8636 ) ;
#2725 = EDGE_LOOP ( 'NONE', ( #3624, #14962, #6912, #14335 ) ) ;
#2726 = EDGE_CURVE ( 'NONE', #2157, #15536, #7207, .T. ) ;
#2727 = DIRECTION ( 'NONE',  ( -1.000000000000000000, 0.000000000000000000, 0.000000000000000000 ) ) ;
#2728 = FILL_AREA_STYLE_COLOUR ( '', #8034 ) ;
#2729 = ADVANCED_FACE ( 'NONE', ( #12845 ), #9883, .T. ) ;
#2730 = ADVANCED_FACE ( 'NONE', ( #3029 ), #1402, .T. ) ;
#2731 = ORIENTED_EDGE ( 'NONE', *, *, #14036, .T. ) ;
#2732 = DIRECTION ( 'NONE',  ( 0.000000000000000000, 0.000000000000000000, 1.000000000000000000 ) ) ;
#2733 = TOROIDAL_SURFACE ( 'NONE', #1515, 29.90000000000000213, 0.1000000000000011297 ) ;
#2734 = AXIS2_PLACEMENT_3D ( 'NONE', #7834, #793, #12213 ) ;
#2735 = EDGE_CURVE ( 'NONE', #2861, #17956, #13669, .T. ) ;
#2736 = FACE_BOUND ( 'NONE', #8126, .T. ) ;
#2737 = DIRECTION ( 'NONE',  ( 0.000000000000000000, 0.000000000000000000, 1.000000000000000000 ) ) ;
#2738 = EDGE_LOOP ( 'NONE', ( #9733, #12727, #5582, #3284 ) ) ;
#2739 = CARTESIAN_POINT ( 'NONE',  ( 10.00000000000000000, 24.97244012287502102, 57.83923611457328207 ) ) ;
#2740 = EDGE_CURVE ( 'NONE', #13520, #5686, #5697, .T. ) ;
#2741 = VECTOR ( 'NONE', #9770, 1000.000000000000000 ) ;
#2742 = ORIENTED_EDGE ( 'NONE', *, *, #10162, .F. ) ;
#2743 = UNCERTAINTY_MEASURE_WITH_UNIT (LENGTH_MEASURE( 1.000000000000000082E-05 ), #3690, 'distance_accuracy_value', 'NONE');
#2744 = CARTESIAN_POINT ( 'NONE',  ( 21.00000000000000000, 2.055000000000000160, 0.000000000000000000 ) ) ;
#2745 = ORIENTED_EDGE ( 'NONE', *, *, #16920, .F. ) ;
#2746 = CARTESIAN_POINT ( 'NONE',  ( -4.000000000000000000, -7.806255641895631925E-15, -3.142992957459232350 ) ) ;
#2747 = EDGE_LOOP ( 'NONE', ( #10709, #12559 ) ) ;
#2748 = AXIS2_PLACEMENT_3D ( 'NONE', #225, #8696, #5927 ) ;
#2749 = DIRECTION ( 'NONE',  ( -1.000000000000000000, -0.000000000000000000, 0.000000000000000000 ) ) ;
#2750 = CARTESIAN_POINT ( 'NONE',  ( 1.393927851585479161, -4.043713361053543842, -3.526374918436840922 ) ) ;
#2751 = ORIENTED_EDGE ( 'NONE', *, *, #4432, .F. ) ;
#2752 = ORIENTED_EDGE ( 'NONE', *, *, #938, .T. ) ;
#2753 = ADVANCED_FACE ( 'NONE', ( #17223 ), #2649, .T. ) ;
#2754 = DIRECTION ( 'NONE',  ( 0.000000000000000000, 1.000000000000000000, 0.000000000000000000 ) ) ;
#2755 = ORIENTED_EDGE ( 'NONE', *, *, #12199, .F. ) ;
#2756 = CARTESIAN_POINT ( 'NONE',  ( 10.00000000000000000, 32.11449294037196012, 54.20017844242522642 ) ) ;
#2757 = DIRECTION ( 'NONE',  ( 0.000000000000000000, 0.000000000000000000, 1.000000000000000000 ) ) ;
#2758 = AXIS2_PLACEMENT_3D ( 'NONE', #12017, #16041, #13100 ) ;
#2759 = EDGE_CURVE ( 'NONE', #125, #13093, #581, .T. ) ;
#2760 = VECTOR ( 'NONE', #6122, 1000.000000000000000 ) ;
#2761 = FACE_OUTER_BOUND ( 'NONE', #9221, .T. ) ;
#2762 = VERTEX_POINT ( 'NONE', #10163 ) ;
#2763 = ORIENTED_EDGE ( 'NONE', *, *, #14780, .F. ) ;
#2764 = LINE ( 'NONE', #12948, #2941 ) ;
#2765 = DIRECTION ( 'NONE',  ( 0.000000000000000000, 0.000000000000000000, 1.000000000000000000 ) ) ;
#2766 = DIRECTION ( 'NONE',  ( -1.000000000000000000, 0.000000000000000000, -0.000000000000000000 ) ) ;
#2767 = CARTESIAN_POINT ( 'NONE',  ( -4.203934362469166963, -1.640673743454851286, -3.598432614606932756 ) ) ;
#2768 = DIRECTION ( 'NONE',  ( 0.000000000000000000, 0.000000000000000000, 1.000000000000000000 ) ) ;
#2769 = CARTESIAN_POINT ( 'NONE',  ( 2.354826896168714434, -6.962563485461402024, -1.000000000000000000 ) ) ;
#2770 = DIRECTION ( 'NONE',  ( 0.000000000000000000, 1.000000000000000000, 0.000000000000000000 ) ) ;
#2771 = ORIENTED_EDGE ( 'NONE', *, *, #13030, .F. ) ;
#2772 = DIRECTION ( 'NONE',  ( -1.000000000000000000, -0.000000000000000000, -0.000000000000000000 ) ) ;
#2773=STYLED_ITEM('',(#18855),#10108);
#2774 = FACE_OUTER_BOUND ( 'NONE', #18273, .T. ) ;
#2775 = ORIENTED_EDGE ( 'NONE', *, *, #2348, .T. ) ;
#2776 = PLANE ( 'NONE',  #879 ) ;
#2777 = DIRECTION ( 'NONE',  ( 0.000000000000000000, 0.000000000000000000, 1.000000000000000000 ) ) ;
#2778 = ORIENTED_EDGE ( 'NONE', *, *, #402, .T. ) ;
#2779 = ADVANCED_FACE ( 'NONE', ( #11603 ), #15798, .T. ) ;
#2780 = ORIENTED_EDGE ( 'NONE', *, *, #12189, .T. ) ;
#2781 = AXIS2_PLACEMENT_3D ( 'NONE', #823, #5190, #6345 ) ;
#2782 = FACE_OUTER_BOUND ( 'NONE', #15214, .T. ) ;
#2783 = DIRECTION ( 'NONE',  ( -1.000000000000000000, 0.000000000000000000, -0.000000000000000000 ) ) ;
#2784 = VERTEX_POINT ( 'NONE', #8463 ) ;
#2785 = B_SPLINE_CURVE_WITH_KNOTS ( 'NONE', 3,
 ( #4840, #6164, #12169, #16261, #17977, #358 ),
 .UNSPECIFIED., .F., .F.,
 ( 4, 2, 4 ),
 ( -3.640115492410698714E-06, 0.0002066546034003381217, 0.0004169493222930869755 ),
 .UNSPECIFIED. ) ;
#2786 = CARTESIAN_POINT ( 'NONE',  ( 4.000000000000000000, 0.9868501483902631932, -0.09357334158579604100 ) ) ;
#2787 = CYLINDRICAL_SURFACE ( 'NONE', #1457, 2.649999999999992806 ) ;
#2788 = DIRECTION ( 'NONE',  ( 0.000000000000000000, 0.000000000000000000, 1.000000000000000000 ) ) ;
#2789 = FACE_OUTER_BOUND ( 'NONE', #15795, .T. ) ;
#2790 = EDGE_LOOP ( 'NONE', ( #1972, #4474, #11804 ) ) ;
#2791 = FACE_OUTER_BOUND ( 'NONE', #2398, .T. ) ;
#2792 = ORIENTED_EDGE ( 'NONE', *, *, #270, .T. ) ;
#2793 = ADVANCED_FACE ( 'NONE', ( #15885 ), #10256, .T. ) ;
#2794 = SURFACE_STYLE_USAGE ( .BOTH. , #11462 ) ;
#2795 = CARTESIAN_POINT ( 'NONE',  ( 10.00000000000000000, 0.000000000000000000, 0.000000000000000000 ) ) ;
#2796 = ORIENTED_EDGE ( 'NONE', *, *, #13436, .T. ) ;
#2797 = PRODUCT_CONTEXT ( 'NONE', #8284, 'mechanical' ) ;
#2798 = ADVANCED_FACE ( 'NONE', ( #18561 ), #14279, .T. ) ;
#2799 = DIRECTION ( 'NONE',  ( 1.000000000000000000, 0.000000000000000000, 0.000000000000000000 ) ) ;
#2800 = VERTEX_POINT ( 'NONE', #9981 ) ;
#2801 = CIRCLE ( 'NONE', #12208, 150.0000000000000000 ) ;
#2802 = AXIS2_PLACEMENT_3D ( 'NONE', #11320, #18569, #11029 ) ;
#2803 = PLANE ( 'NONE',  #1105 ) ;
#2804 = CARTESIAN_POINT ( 'NONE',  ( 45.00000000000000000, 10.00000000000000000, 2.649999999999487432 ) ) ;
#2805 = DIRECTION ( 'NONE',  ( 1.000000000000000000, 0.000000000000000000, 0.000000000000000000 ) ) ;
#2806 = DIRECTION ( 'NONE',  ( -1.000000000000000000, 0.000000000000000000, -0.000000000000000000 ) ) ;
#2807 = CIRCLE ( 'NONE', #5228, 24.00000000002399858 ) ;
#2808 = DIRECTION ( 'NONE',  ( 1.000000000000000000, -2.031314180040284764E-16, 0.000000000000000000 ) ) ;
#2809 = EDGE_LOOP ( 'NONE', ( #7698, #6529, #4423, #498 ) ) ;
#2810 = AXIS2_PLACEMENT_3D ( 'NONE', #16094, #10183, #1803 ) ;
#2811 = CARTESIAN_POINT ( 'NONE',  ( -12.50000000000000355, 0.000000000000000000, -27.00000000000000355 ) ) ;
#2812 = LINE ( 'NONE', #2722, #12897 ) ;
#2813 = FACE_OUTER_BOUND ( 'NONE', #12249, .T. ) ;
#2814 = ORIENTED_EDGE ( 'NONE', *, *, #6913, .F. ) ;
#2815 = ORIENTED_EDGE ( 'NONE', *, *, #13104, .T. ) ;
#2816 = DIRECTION ( 'NONE',  ( 0.000000000000000000, -1.000000000000000000, 0.000000000000000000 ) ) ;
#2817 = PRESENTATION_STYLE_ASSIGNMENT (( #63 ) ) ;
#2818 = VERTEX_POINT ( 'NONE', #1503 ) ;
#2819 = PRODUCT_DEFINITION_SHAPE ( 'NONE', 'NONE',  #18811 ) ;
#2820 = AXIS2_PLACEMENT_3D ( 'NONE', #4849, #11979, #10654 ) ;
#2821 = DIRECTION ( 'NONE',  ( 0.000000000000000000, -1.000000000000000000, 0.000000000000000000 ) ) ;
#2822 = VECTOR ( 'NONE', #1032, 1000.000000000000000 ) ;
#2823 = VECTOR ( 'NONE', #17528, 1000.000000000000000 ) ;
#2824 = FACE_OUTER_BOUND ( 'NONE', #16537, .T. ) ;
#2825 = ADVANCED_FACE ( 'NONE', ( #5792 ), #4360, .F. ) ;
#2826 = ORIENTED_EDGE ( 'NONE', *, *, #5762, .F. ) ;
#2827 = EDGE_CURVE ( 'NONE', #16722, #5310, #4082, .T. ) ;
#2828 = EDGE_CURVE ( 'NONE', #8859, #15153, #14572, .T. ) ;
#2829 = ORIENTED_EDGE ( 'NONE', *, *, #16831, .T. ) ;
#2830 = DIRECTION ( 'NONE',  ( 1.000000000000000000, 0.000000000000000000, 0.000000000000000000 ) ) ;
#2831 = ORIENTED_EDGE ( 'NONE', *, *, #4665, .T. ) ;
#2832 = DIRECTION ( 'NONE',  ( 0.000000000000000000, 0.000000000000000000, 1.000000000000000000 ) ) ;
#2833 = VERTEX_POINT ( 'NONE', #17327 ) ;
#2834 = ADVANCED_FACE ( 'NONE', ( #10713 ), #14924, .F. ) ;
#2835 = CARTESIAN_POINT ( 'NONE',  ( 10.00000000000000000, 1.335003989221626997, 56.23315539212691050 ) ) ;
#2836 = CARTESIAN_POINT ( 'NONE',  ( 10.00000000000000000, 0.000000000000000000, 0.000000000000000000 ) ) ;
#2837 = EDGE_LOOP ( 'NONE', ( #14120, #10715 ) ) ;
#2838 = ORIENTED_EDGE ( 'NONE', *, *, #5867, .T. ) ;
#2839 = CYLINDRICAL_SURFACE ( 'NONE', #5691, 24.00000000002399858 ) ;
#2840 =( LENGTH_UNIT ( ) NAMED_UNIT ( * ) SI_UNIT ( .MILLI., .METRE. ) );
#2841 = EDGE_CURVE ( 'NONE', #17054, #5933, #17019, .T. ) ;
#2842 = AXIS2_PLACEMENT_3D ( 'NONE', #638, #2156, #16353 ) ;
#2843 = VERTEX_POINT ( 'NONE', #1590 ) ;
#2844 = CARTESIAN_POINT ( 'NONE',  ( 10.00000000000000000, 27.72801475327282361, -5.086963483077305170 ) ) ;
#2845 = AXIS2_PLACEMENT_3D ( 'NONE', #15238, #14861, #10564 ) ;
#2846 = ADVANCED_FACE ( 'NONE', ( #17872 ), #16535, .F. ) ;
#2847 = CYLINDRICAL_SURFACE ( 'NONE', #676, 27.29487558977753991 ) ;
#2848 = ORIENTED_EDGE ( 'NONE', *, *, #12889, .F. ) ;
#2849 = EDGE_CURVE ( 'NONE', #18692, #2244, #16352, .T. ) ;
#2850 = AXIS2_PLACEMENT_3D ( 'NONE', #10051, #5773, #14705 ) ;
#2851 = ADVANCED_FACE ( 'NONE', ( #3397 ), #4828, .T. ) ;
#2852 = ORIENTED_EDGE ( 'NONE', *, *, #16913, .T. ) ;
#2853 = CYLINDRICAL_SURFACE ( 'NONE', #11146, 63.00000000006298961 ) ;
#2854 = CARTESIAN_POINT ( 'NONE',  ( -117.1020693116508085, -30.00000000000000000, 22.34080595179776907 ) ) ;
#2855 = FACE_OUTER_BOUND ( 'NONE', #14001, .T. ) ;
#2856 = PLANE ( 'NONE',  #11771 ) ;
#2857 = CARTESIAN_POINT ( 'NONE',  ( -4.000000000000000000, -2.512220745329312610, -3.469390707569719901 ) ) ;
#2858 = CARTESIAN_POINT ( 'NONE',  ( 10.00000000000000000, 0.000000000000000000, 0.000000000000000000 ) ) ;
#2859 = DIRECTION ( 'NONE',  ( -1.000000000000000000, 0.000000000000000000, 0.000000000000000000 ) ) ;
#2860 = CARTESIAN_POINT ( 'NONE',  ( -1.144235203016679359, -3.958177651039096911, -0.09382832055446428676 ) ) ;
#2861 = VERTEX_POINT ( 'NONE', #10629 ) ;
#2862 = DIRECTION ( 'NONE',  ( 0.000000000000000000, 0.000000000000000000, 1.000000000000000000 ) ) ;
#2863 = EDGE_CURVE ( 'NONE', #16191, #5775, #6889, .T. ) ;
#2864 = CARTESIAN_POINT ( 'NONE',  ( 2.449293598294706513E-15, -34.99999999999999289, -20.00000000000000000 ) ) ;
#2865 = EDGE_CURVE ( 'NONE', #9332, #13562, #14637, .T. ) ;
#2866 = ORIENTED_EDGE ( 'NONE', *, *, #2302, .F. ) ;
#2867 = CARTESIAN_POINT ( 'NONE',  ( -0.1481481481481481122, -4.797713218419819903, -1.000000000000000000 ) ) ;
#2868 = CARTESIAN_POINT ( 'NONE',  ( 129.9999999999999432, -34.99999999999999289, -125.0000000000000000 ) ) ;
#2869 = CIRCLE ( 'NONE', #17462, 24.00000000002399858 ) ;
#2870 = ORIENTED_EDGE ( 'NONE', *, *, #17509, .T. ) ;
#2871 = ORIENTED_EDGE ( 'NONE', *, *, #18298, .T. ) ;
#2872 = CYLINDRICAL_SURFACE ( 'NONE', #6888, 63.00000000006298961 ) ;
#2873 = LINE ( 'NONE', #14487, #337 ) ;
#2874 = ORIENTED_EDGE ( 'NONE', *, *, #16364, .F. ) ;
#2875 = SURFACE_STYLE_USAGE ( .BOTH. , #11552 ) ;
#2876 = LINE ( 'NONE', #11553, #2632 ) ;
#2877 = PRESENTATION_LAYER_ASSIGNMENT (  '', '', ( #5608 ) ) ;
#2878 = CARTESIAN_POINT ( 'NONE',  ( 2.500000000000000000, 1.178949249685213863, -2.042000000000001148 ) ) ;
#2879 = CARTESIAN_POINT ( 'NONE',  ( 10.00000000000000000, -58.55669782892444175, -23.24033432160499757 ) ) ;
#2880 = ORIENTED_EDGE ( 'NONE', *, *, #16473, .F. ) ;
#2881 = CARTESIAN_POINT ( 'NONE',  ( -26.29305231718568336, -30.00000000000000000, -19.10302069950552095 ) ) ;
#2882 = ORIENTED_EDGE ( 'NONE', *, *, #17547, .T. ) ;
#2883 = ADVANCED_FACE ( 'NONE', ( #10436 ), #4542, .F. ) ;
#2884 = FACE_OUTER_BOUND ( 'NONE', #6510, .T. ) ;
#2885 = DIRECTION ( 'NONE',  ( -0.000000000000000000, 1.000000000000000000, -0.000000000000000000 ) ) ;
#2886 = ORIENTED_EDGE ( 'NONE', *, *, #17266, .F. ) ;
#2887 = CONTEXT_DEPENDENT_SHAPE_REPRESENTATION ( #6103, #4503 ) ;
#2888 = ORIENTED_EDGE ( 'NONE', *, *, #17161, .F. ) ;
#2889 = CIRCLE ( 'NONE', #5317, 56.24900000005627021 ) ;
#2890 = AXIS2_PLACEMENT_3D ( 'NONE', #11013, #9499, #3505 ) ;
#2891 = EDGE_CURVE ( 'NONE', #3956, #15653, #1868, .T. ) ;
#2892 = DIRECTION ( 'NONE',  ( 0.000000000000000000, 0.000000000000000000, 1.000000000000000000 ) ) ;
#2893 = DIRECTION ( 'NONE',  ( 0.000000000000000000, 0.000000000000000000, -1.000000000000000000 ) ) ;
#2894 = DIRECTION ( 'NONE',  ( -1.000000000000000000, 0.000000000000000000, 0.000000000000000000 ) ) ;
#2895 = CARTESIAN_POINT ( 'NONE',  ( 2.449293598294706513E-15, 15.00000000000000000, -20.00000000000000000 ) ) ;
#2896 = EDGE_CURVE ( 'NONE', #12127, #7525, #12044, .T. ) ;
#2897 = CARTESIAN_POINT ( 'NONE',  ( 10.00000000000000000, -16.60877409751182654, 20.32630374611179391 ) ) ;
#2898 = ORIENTED_EDGE ( 'NONE', *, *, #3368, .F. ) ;
#2899 = ORIENTED_EDGE ( 'NONE', *, *, #15271, .F. ) ;
#2900 = AXIS2_PLACEMENT_3D ( 'NONE', #3477, #9373, #915 ) ;
#2901 = DIRECTION ( 'NONE',  ( -1.000000000000000000, -0.000000000000000000, 0.000000000000000000 ) ) ;
#2902 = FACE_OUTER_BOUND ( 'NONE', #17979, .T. ) ;
#2903 = CARTESIAN_POINT ( 'NONE',  ( 6.735557395310442615E-15, 0.000000000000000000, 55.00000000000000000 ) ) ;
#2904 = EDGE_LOOP ( 'NONE', ( #3062, #8872 ) ) ;
#2905 = VECTOR ( 'NONE', #17759, 1000.000000000000000 ) ;
#2906 = ORIENTED_EDGE ( 'NONE', *, *, #5226, .F. ) ;
#2907 = CIRCLE ( 'NONE', #17203, 30.00000000000000711 ) ;
#2908 = CARTESIAN_POINT ( 'NONE',  ( 10.00000000000000000, 56.37237871411034007, 1.017308535512583711 ) ) ;
#2909 = ORIENTED_EDGE ( 'NONE', *, *, #18022, .F. ) ;
#2910 = VECTOR ( 'NONE', #11965, 1000.000000000000000 ) ;
#2911 = DIRECTION ( 'NONE',  ( 0.8660254037844379305, 0.5000000000000013323, 0.000000000000000000 ) ) ;
#2912 = CARTESIAN_POINT ( 'NONE',  ( 0.000000000000000000, 0.000000000000000000, 0.000000000000000000 ) ) ;
#2913 = AXIS2_PLACEMENT_3D ( 'NONE', #6516, #7946, #6621 ) ;
#2915 = AXIS2_PLACEMENT_3D ( 'NONE', #11642, #13079, #11913 ) ;
#2914 = DIRECTION ( 'NONE',  ( -1.000000000000000000, 0.000000000000000000, 0.000000000000000000 ) ) ;
#2916 = VERTEX_POINT ( 'NONE', #9194 ) ;
#2917 = CARTESIAN_POINT ( 'NONE',  ( 0.000000000000000000, -24.68609584167194981, 50.69000562871634230 ) ) ;
#2918 = ORIENTED_EDGE ( 'NONE', *, *, #18618, .T. ) ;
#2919 = LINE ( 'NONE', #8726, #13319 ) ;
#2920 = ORIENTED_EDGE ( 'NONE', *, *, #9059, .F. ) ;
#2921 = ORIENTED_EDGE ( 'NONE', *, *, #2579, .F. ) ;
#2922 = CARTESIAN_POINT ( 'NONE',  ( 34.55500000000001393, 0.000000000000000000, 0.000000000000000000 ) ) ;
#2923 = LINE ( 'NONE', #14544, #7380 ) ;
#2924 = AXIS2_PLACEMENT_3D ( 'NONE', #6711, #3754, #18037 ) ;
#2925 = ORIENTED_EDGE ( 'NONE', *, *, #496, .F. ) ;
#2926 = ORIENTED_EDGE ( 'NONE', *, *, #17885, .F. ) ;
#2927 = VECTOR ( 'NONE', #13281, 1000.000000000000000 ) ;
#2928 = FACE_OUTER_BOUND ( 'NONE', #4526, .T. ) ;
#2929 =( LENGTH_UNIT ( ) NAMED_UNIT ( * ) SI_UNIT ( .MILLI., .METRE. ) );
#2930 = VECTOR ( 'NONE', #505, 1000.000000000000000 ) ;
#2931 = EDGE_LOOP ( 'NONE', ( #11354, #3267, #8279, #6111 ) ) ;
#2932 = DIRECTION ( 'NONE',  ( -0.000000000000000000, 1.000000000000000000, -0.000000000000000000 ) ) ;
#2933 = CIRCLE ( 'NONE', #16607, 26.24900000002625333 ) ;
#2934 = AXIS2_PLACEMENT_3D ( 'NONE', #9482, #13856, #829 ) ;
#2935 = CIRCLE ( 'NONE', #494, 8.099999999999999645 ) ;
#2936 = ADVANCED_FACE ( 'NONE', ( #3116 ), #11961, .T. ) ;
#2937 = ADVANCED_FACE ( 'NONE', ( #14727 ), #7487, .T. ) ;
#2938 = APPLICATION_CONTEXT ( 'automotive_design' ) ;
#2939 = PRODUCT_RELATED_PRODUCT_CATEGORY ( 'part', '', ( #8595 ) ) ;
#2940 = CARTESIAN_POINT ( 'NONE',  ( 0.000000000000000000, 0.000000000000000000, 0.000000000000000000 ) ) ;
#2941 = VECTOR ( 'NONE', #5714, 1000.000000000000000 ) ;
#2942 = MECHANICAL_DESIGN_GEOMETRIC_PRESENTATION_REPRESENTATION (  '', ( #18751 ), #11458 ) ;
#2943 = ORIENTED_EDGE ( 'NONE', *, *, #9943, .T. ) ;
#2944 = EDGE_CURVE ( 'NONE', #15698, #10240, #10229, .T. ) ;
#2945 = AXIS2_PLACEMENT_3D ( 'NONE', #17447, #8680, #8948 ) ;
#2946 = CIRCLE ( 'NONE', #3547, 2.649999999999999467 ) ;
#2947 = ORIENTED_EDGE ( 'NONE', *, *, #10834, .F. ) ;
#2948 = CARTESIAN_POINT ( 'NONE',  ( -2.250000000000000000, -27.60846790388774608, 0.000000000000000000 ) ) ;
#2949 = VECTOR ( 'NONE', #11136, 1000.000000000000000 ) ;
#2950 = DIRECTION ( 'NONE',  ( -1.000000000000000000, -0.000000000000000000, 0.000000000000000000 ) ) ;
#2951 = DIRECTION ( 'NONE',  ( 0.000000000000000000, 0.000000000000000000, 1.000000000000000000 ) ) ;
#2952 = DIRECTION ( 'NONE',  ( -1.000000000000000000, 0.000000000000000000, 0.000000000000000000 ) ) ;
#2953 = DIRECTION ( 'NONE',  ( 0.000000000000000000, -0.8090169943749532244, 0.5877852522924652545 ) ) ;
#2954 = EDGE_CURVE ( 'NONE', #3496, #10145, #7497, .T. ) ;
#2955 = CARTESIAN_POINT ( 'NONE',  ( 10.00000000000000000, 0.000000000000000000, 0.000000000000000000 ) ) ;
#2956 = CARTESIAN_POINT ( 'NONE',  ( 0.000000000000000000, 0.000000000000000000, 0.000000000000000000 ) ) ;
#2957 = CARTESIAN_POINT ( 'NONE',  ( -0.3198814748697807464, -4.434118497892185040, -0.3507732604232532969 ) ) ;
#2958 = VERTEX_POINT ( 'NONE', #7584 ) ;
#2959 = CARTESIAN_POINT ( 'NONE',  ( 3.098410542199072637, -7.060458129626440815, -1.000000000000000000 ) ) ;
#2960 = DIRECTION ( 'NONE',  ( 0.000000000000000000, 0.000000000000000000, 1.000000000000000000 ) ) ;
#2961 = ORIENTED_EDGE ( 'NONE', *, *, #5295, .T. ) ;
#2962 = CARTESIAN_POINT ( 'NONE',  ( 0.000000000000000000, 27.72801475327282361, -5.086963483077305170 ) ) ;
#2963 = FACE_BOUND ( 'NONE', #3551, .T. ) ;
#2964 = VECTOR ( 'NONE', #9303, 1000.000000000000000 ) ;
#2965 = ADVANCED_FACE ( 'NONE', ( #12156 ), #4916, .T. ) ;
#2966 = AXIS2_PLACEMENT_3D ( 'NONE', #949, #8074, #6938 ) ;
#2967 = ADVANCED_FACE ( 'NONE', ( #12053 ), #8154, .T. ) ;
#2968 = VECTOR ( 'NONE', #18162, 1000.000000000000000 ) ;
#2969 = VECTOR ( 'NONE', #4414, 1000.000000000000114 ) ;
#2970 = ADVANCED_FACE ( 'NONE', ( #3592 ), #731, .T. ) ;
#2971 = EDGE_CURVE ( 'NONE', #17712, #12431, #4166, .T. ) ;
#2972 = ORIENTED_EDGE ( 'NONE', *, *, #2579, .T. ) ;
#2973 = DIRECTION ( 'NONE',  ( -1.000000000000000000, -0.000000000000000000, -0.000000000000000000 ) ) ;
#2974 = DIRECTION ( 'NONE',  ( -0.000000000000000000, -1.000000000000000000, -0.000000000000000000 ) ) ;
#2975 = AXIS2_PLACEMENT_3D ( 'NONE', #2744, #5690, #3026 ) ;
#2976 = ORIENTED_EDGE ( 'NONE', *, *, #10641, .T. ) ;
#2977 = DIRECTION ( 'NONE',  ( 1.000000000000000000, 0.000000000000000000, 0.000000000000000000 ) ) ;
#2978 = DIRECTION ( 'NONE',  ( -1.000000000000000000, -0.000000000000000000, -0.000000000000000000 ) ) ;
#2979 = CIRCLE ( 'NONE', #14535, 2.649999999999995914 ) ;
#2980 = EDGE_CURVE ( 'NONE', #10448, #12127, #6441, .T. ) ;
#2981 = CARTESIAN_POINT ( 'NONE',  ( -0.5000000000000000000, -6.429618962271402616, 0.000000000000000000 ) ) ;
#2982 = CYLINDRICAL_SURFACE ( 'NONE', #7655, 2.649999999999999467 ) ;
#2983 = CIRCLE ( 'NONE', #13626, 27.50000000000000000 ) ;
#2984 = FACE_OUTER_BOUND ( 'NONE', #8511, .T. ) ;
#2985 = VERTEX_POINT ( 'NONE', #11192 ) ;
#2986 = CIRCLE ( 'NONE', #13924, 2.649999999999992806 ) ;
#2987 = DIRECTION ( 'NONE',  ( -1.000000000000000000, -0.000000000000000000, -0.000000000000000000 ) ) ;
#2988 = ORIENTED_EDGE ( 'NONE', *, *, #4245, .F. ) ;
#2989 = PRODUCT_DEFINITION_SHAPE ( 'NONE', 'NONE',  #18818 ) ;
#2990 = DIRECTION ( 'NONE',  ( 1.000000000000000000, 0.000000000000000000, 0.000000000000000000 ) ) ;
#2991 = CARTESIAN_POINT ( 'NONE',  ( -90.38553543446691663, 1.821459649775647449E-14, -4.784491867360616268 ) ) ;
#2992 = ORIENTED_EDGE ( 'NONE', *, *, #13827, .F. ) ;
#2993 = VERTEX_POINT ( 'NONE', #14055 ) ;
#2994 = AXIS2_PLACEMENT_3D ( 'NONE', #4913, #9192, #6242 ) ;
#2995 = AXIS2_PLACEMENT_3D ( 'NONE', #6407, #13467, #504 ) ;
#2996 = EDGE_CURVE ( 'NONE', #15825, #6010, #809, .T. ) ;
#2997 = DIRECTION ( 'NONE',  ( -0.000000000000000000, -0.000000000000000000, 1.000000000000000000 ) ) ;
#2998 = FACE_OUTER_BOUND ( 'NONE', #18263, .T. ) ;
#2999 = FACE_OUTER_BOUND ( 'NONE', #10741, .T. ) ;
#3000 = DIRECTION ( 'NONE',  ( 0.000000000000000000, 0.000000000000000000, 1.000000000000000000 ) ) ;
#3001 = CARTESIAN_POINT ( 'NONE',  ( -0.6507732100473471171, 4.243078065514775510, -0.2236248678334823436 ) ) ;
#3002 = VECTOR ( 'NONE', #17940, 1000.000000000000000 ) ;
#3003 = CARTESIAN_POINT ( 'NONE',  ( 0.000000000000000000, -1.178949249685214307, 2.042000000000001592 ) ) ;
#3004 = DIRECTION ( 'NONE',  ( -1.000000000000000000, 0.000000000000000000, 0.000000000000000000 ) ) ;
#3005 = EDGE_LOOP ( 'NONE', ( #108, #11824 ) ) ;
#3006 = CIRCLE ( 'NONE', #17900, 12.00000000001200640 ) ;
#3007 = CARTESIAN_POINT ( 'NONE',  ( 10.00000000000000178, 3.673940397442059178E-15, -30.00000000000000000 ) ) ;
#3008 = DIRECTION ( 'NONE',  ( 0.000000000000000000, 0.000000000000000000, 1.000000000000000000 ) ) ;
#3009 = CYLINDRICAL_SURFACE ( 'NONE', #15827, 2.649999999999999467 ) ;
#3010 = VECTOR ( 'NONE', #5639, 1000.000000000000000 ) ;
#3011 = EDGE_LOOP ( 'NONE', ( #13175, #12108, #8959, #12733 ) ) ;
#3012 = VERTEX_POINT ( 'NONE', #18427 ) ;
#3013 = CIRCLE ( 'NONE', #18523, 26.24900000002625688 ) ;
#3014 = CARTESIAN_POINT ( 'NONE',  ( -90.00000000009001155, -34.99999999999999289, -1.301042606982603940E-15 ) ) ;
#3015 = ORIENTED_EDGE ( 'NONE', *, *, #2001, .F. ) ;
#3016 = AXIS2_PLACEMENT_3D ( 'NONE', #12218, #993, #8022 ) ;
#3017 = EDGE_CURVE ( 'NONE', #9182, #10921, #3548, .T. ) ;
#3018 = CIRCLE ( 'NONE', #17613, 2.649999999999992806 ) ;
#3019 = CARTESIAN_POINT ( 'NONE',  ( 10.04305231718579705, -26.50000000000000000, 28.25933677959249835 ) ) ;
#3020 = FACE_OUTER_BOUND ( 'NONE', #10431, .T. ) ;
#3021 = AXIS2_PLACEMENT_3D ( 'NONE', #10352, #13407, #1958 ) ;
#3022 = CARTESIAN_POINT ( 'NONE',  ( 0.000000000000000000, -13.75000000000000355, 0.000000000000000000 ) ) ;
#3023 = ORIENTED_EDGE ( 'NONE', *, *, #4574, .F. ) ;
#3024 = CARTESIAN_POINT ( 'NONE',  ( 0.000000000000000000, 9.823366686500662581, 55.51919907100656104 ) ) ;
#3025 = ORIENTED_EDGE ( 'NONE', *, *, #8650, .T. ) ;
#3026 = DIRECTION ( 'NONE',  ( 0.000000000000000000, 0.000000000000000000, -1.000000000000000000 ) ) ;
#3027 = ORIENTED_EDGE ( 'NONE', *, *, #6680, .F. ) ;
#3028 = ORIENTED_EDGE ( 'NONE', *, *, #6845, .T. ) ;
#3029 = FACE_OUTER_BOUND ( 'NONE', #5506, .T. ) ;
#3030 = DIRECTION ( 'NONE',  ( -1.000000000000000000, 0.000000000000000000, 0.000000000000000000 ) ) ;
#3031 = ORIENTED_EDGE ( 'NONE', *, *, #9947, .F. ) ;
#3032 = ORIENTED_EDGE ( 'NONE', *, *, #15524, .F. ) ;
#3033 = EDGE_CURVE ( 'NONE', #11704, #15321, #9938, .T. ) ;
#3034 = CARTESIAN_POINT ( 'NONE',  ( 10.00000000000000000, 0.000000000000000000, 0.000000000000000000 ) ) ;
#3035 = CONICAL_SURFACE ( 'NONE', #10930, 4.000000000000000000, 0.8911886515913786111 ) ;
#3036 =( NAMED_UNIT ( * ) PLANE_ANGLE_UNIT ( ) SI_UNIT ( $, .RADIAN. ) );
#3037 = ORIENTED_EDGE ( 'NONE', *, *, #681, .T. ) ;
#3038 = CARTESIAN_POINT ( 'NONE',  ( -79.64793068852927149, -38.00000000000000000, 31.86039329588764701 ) ) ;
#3039 = EDGE_CURVE ( 'NONE', #6042, #6241, #12334, .T. ) ;
#3040 = CYLINDRICAL_SURFACE ( 'NONE', #4626, 33.00000000003299760 ) ;
#3041 = CIRCLE ( 'NONE', #5481, 24.00000000002399858 ) ;
#3042 = ORIENTED_EDGE ( 'NONE', *, *, #6050, .T. ) ;
#3043 = AXIS2_PLACEMENT_3D ( 'NONE', #16223, #7277, #47 ) ;
#3044 = EDGE_LOOP ( 'NONE', ( #1083, #17491, #12330, #6547 ) ) ;
#3045 = DIRECTION ( 'NONE',  ( -1.000000000000000000, -0.000000000000000000, -0.000000000000000000 ) ) ;
#3046 = CARTESIAN_POINT ( 'NONE',  ( 10.00000000000000000, -6.681932690256794594, -25.38428207620328791 ) ) ;
#3047 = LINE ( 'NONE', #5894, #5084 ) ;
#3048 = VERTEX_POINT ( 'NONE', #13772 ) ;
#3049 = CARTESIAN_POINT ( 'NONE',  ( 10.00000000000000000, 16.60877409751197575, -20.32630374611166957 ) ) ;
#3050 = DIRECTION ( 'NONE',  ( 1.000000000000000000, 0.000000000000000000, 0.000000000000000000 ) ) ;
#3051 = CARTESIAN_POINT ( 'NONE',  ( 5.560781378645575757, 0.000000000000000000, -4.000000000000000000 ) ) ;
#3052 = DIRECTION ( 'NONE',  ( 0.000000000000000000, 0.000000000000000000, 1.000000000000000000 ) ) ;
#3053 = ORIENTED_EDGE ( 'NONE', *, *, #15279, .F. ) ;
#3054 = CARTESIAN_POINT ( 'NONE',  ( 0.000000000000000000, -49.49802920186242261, 26.71881558261711831 ) ) ;
#3055 = DIRECTION ( 'NONE',  ( 0.000000000000000000, -6.938893903900287191E-15, 1.000000000000000000 ) ) ;
#3056 = VERTEX_POINT ( 'NONE', #13688 ) ;
#3057 = DIRECTION ( 'NONE',  ( 0.000000000000000000, 0.000000000000000000, -1.000000000000000000 ) ) ;
#3058 = CARTESIAN_POINT ( 'NONE',  ( 10.00000000000000000, 31.97297851452492168, -46.27827401617368963 ) ) ;
#3059 = CIRCLE ( 'NONE', #10349, 23.50000000000001066 ) ;
#3060 = CIRCLE ( 'NONE', #10663, 24.00000000002400569 ) ;
#3061 = EDGE_CURVE ( 'NONE', #6013, #17928, #14779, .T. ) ;
#3062 = ORIENTED_EDGE ( 'NONE', *, *, #5986, .T. ) ;
#3063 = LINE ( 'NONE', #15222, #3877 ) ;
#3064 = CARTESIAN_POINT ( 'NONE',  ( -2.354826896168714434, -6.962563485461402024, -1.000000000000000000 ) ) ;
#3065 = ORIENTED_EDGE ( 'NONE', *, *, #14566, .F. ) ;
#3066 = CARTESIAN_POINT ( 'NONE',  ( 10.00000000000000000, 46.27827401617449965, -31.97297851452373507 ) ) ;
#3067 = EDGE_CURVE ( 'NONE', #12641, #10237, #8048, .T. ) ;
#3068 = CARTESIAN_POINT ( 'NONE',  ( 5.000000000000000000, -58.55669782892444886, -23.24033432160501178 ) ) ;
#3069 = EDGE_CURVE ( 'NONE', #5083, #18009, #8702, .T. ) ;
#3070 = CIRCLE ( 'NONE', #5504, 8.099999999999999645 ) ;
#3071 = ADVANCED_FACE ( 'NONE', ( #12244 ), #13582, .T. ) ;
#3072 = CARTESIAN_POINT ( 'NONE',  ( -90.00000000009001155, -34.99999999999999289, -40.00000000000000000 ) ) ;
#3073 = CARTESIAN_POINT ( 'NONE',  ( -10.00000000000000000, 26.45033635316149301, 36.40576474687247099 ) ) ;
#3074 = DIRECTION ( 'NONE',  ( 1.000000000000000000, -0.000000000000000000, 0.000000000000000000 ) ) ;
#3075 = ORIENTED_EDGE ( 'NONE', *, *, #5533, .T. ) ;
#3076 = CARTESIAN_POINT ( 'NONE',  ( 10.00000000000000000, -25.38428207620327370, 6.681932690256871865 ) ) ;
#3077 = ORIENTED_EDGE ( 'NONE', *, *, #15484, .T. ) ;
#3078 = EDGE_CURVE ( 'NONE', #11483, #14252, #8058, .T. ) ;
#3079 = PRESENTATION_STYLE_ASSIGNMENT (( #16125 ) ) ;
#3080 = CYLINDRICAL_SURFACE ( 'NONE', #6330, 2.649999999999999467 ) ;
#3081 = ORIENTED_EDGE ( 'NONE', *, *, #6072, .T. ) ;
#3082 = PRODUCT_CONTEXT ( 'NONE', #12791, 'mechanical' ) ;
#3083 = EDGE_LOOP ( 'NONE', ( #1221, #16532, #13684, #14432, #1506, #13517, #11608, #1237 ) ) ;
#3084 = AXIS2_PLACEMENT_3D ( 'NONE', #7754, #7951, #15109 ) ;
#3085 = EDGE_CURVE ( 'NONE', #7671, #6058, #10831, .T. ) ;
#3086 = FACE_OUTER_BOUND ( 'NONE', #13621, .T. ) ;
#3087 = CARTESIAN_POINT ( 'NONE',  ( -56.50000000009000445, -38.00000000000000000, -2.649999999999610889 ) ) ;
#3088 = CYLINDRICAL_SURFACE ( 'NONE', #13932, 63.00000000006298961 ) ;
#3089 = DIRECTION ( 'NONE',  ( 0.000000000000000000, 0.000000000000000000, 1.000000000000000000 ) ) ;
#3090 = ADVANCED_FACE ( 'NONE', ( #5286 ), #12440, .F. ) ;
#3091 = DIRECTION ( 'NONE',  ( -1.000000000000000000, 0.000000000000000000, 0.000000000000000000 ) ) ;
#3092 = CARTESIAN_POINT ( 'NONE',  ( 0.000000000000000000, -40.70683587897930522, -38.81885513160031564 ) ) ;
#3093 = DIRECTION ( 'NONE',  ( 0.000000000000000000, 0.000000000000000000, -1.000000000000000000 ) ) ;
#3094 = ORIENTED_EDGE ( 'NONE', *, *, #18434, .T. ) ;
#3095 = CIRCLE ( 'NONE', #15256, 23.50000000000000355 ) ;
#3096 = LINE ( 'NONE', #3377, #18739 ) ;
#3097 = LINE ( 'NONE', #1482, #113 ) ;
#3098 = CARTESIAN_POINT ( 'NONE',  ( 10.00000000000000000, 23.88582760061481380, 22.76987570971535746 ) ) ;
#3099 = EDGE_LOOP ( 'NONE', ( #3131, #12412, #7674, #13034 ) ) ;
#3100 = VERTEX_POINT ( 'NONE', #12529 ) ;
#3101 = EDGE_CURVE ( 'NONE', #4267, #14062, #5056, .T. ) ;
#3102 = DIRECTION ( 'NONE',  ( 0.000000000000000000, 0.000000000000000000, 1.000000000000000000 ) ) ;
#3103 = FILL_AREA_STYLE ('',( #1303 ) ) ;
#3104 = AXIS2_PLACEMENT_3D ( 'NONE', #12697, #11267, #17089 ) ;
#3105 = FACE_OUTER_BOUND ( 'NONE', #16753, .T. ) ;
#3106 = VERTEX_POINT ( 'NONE', #5671 ) ;
#3107 = CARTESIAN_POINT ( 'NONE',  ( 8.673617379884035472E-16, 4.618802153517012954, 0.000000000000000000 ) ) ;
#3108 = DIRECTION ( 'NONE',  ( 0.000000000000000000, 0.000000000000000000, 1.000000000000000000 ) ) ;
#3109 = AXIS2_PLACEMENT_3D ( 'NONE', #17950, #15475, #8032 ) ;
#3110 = CARTESIAN_POINT ( 'NONE',  ( 0.000000000000000000, -5.086963483077008519, -27.72801475327286980 ) ) ;
#3111 = ORIENTED_EDGE ( 'NONE', *, *, #18029, .F. ) ;
#3112 = PLANE ( 'NONE',  #15248 ) ;
#3113 = VERTEX_POINT ( 'NONE', #8706 ) ;
#3114 = CARTESIAN_POINT ( 'NONE',  ( 10.00000000000000000, -54.20017844242534011, 32.11449294037175406 ) ) ;
#3115 = VERTEX_POINT ( 'NONE', #3969 ) ;
#3116 = FACE_OUTER_BOUND ( 'NONE', #3709, .T. ) ;
#3117 = CARTESIAN_POINT ( 'NONE',  ( 0.3461262719736147297, -4.658553426539303821, -3.671615880910379381 ) ) ;
#3118 = ORIENTED_EDGE ( 'NONE', *, *, #2143, .F. ) ;
#3119 = ORIENTED_EDGE ( 'NONE', *, *, #5107, .F. ) ;
#3120 = EDGE_CURVE ( 'NONE', #18403, #16590, #6572, .T. ) ;
#3121 = DIRECTION ( 'NONE',  ( 0.000000000000000000, 0.000000000000000000, 1.000000000000000000 ) ) ;
#3122 =( NAMED_UNIT ( * ) SI_UNIT ( $, .STERADIAN. ) SOLID_ANGLE_UNIT ( ) );
#3123 = VERTEX_POINT ( 'NONE', #13007 ) ;
#3124 = CARTESIAN_POINT ( 'NONE',  ( 0.000000000000000000, -24.97244012287460535, -57.83923611457346681 ) ) ;
#3125 = VECTOR ( 'NONE', #1591, 1000.000000000000000 ) ;
#3126 = AXIS2_PLACEMENT_3D ( 'NONE', #3946, #13938, #18506 ) ;
#3127 = DIRECTION ( 'NONE',  ( -1.000000000000000000, -0.000000000000000000, -0.000000000000000000 ) ) ;
#3128 = ORIENTED_EDGE ( 'NONE', *, *, #9130, .T. ) ;
#3129 = EDGE_CURVE ( 'NONE', #6635, #12242, #5367, .T. ) ;
#3130 = PRODUCT_DEFINITION_SHAPE ( 'NONE', 'NONE',  #18840 ) ;
#3131 = ORIENTED_EDGE ( 'NONE', *, *, #11068, .T. ) ;
#3132 = DIRECTION ( 'NONE',  ( -1.000000000000000000, -0.000000000000000000, -0.000000000000000000 ) ) ;
#3133 = CARTESIAN_POINT ( 'NONE',  ( -12.69999999999999929, 0.000000000000000000, 0.000000000000000000 ) ) ;
#3134 = DIRECTION ( 'NONE',  ( -1.000000000000000000, -0.000000000000000000, 0.000000000000000000 ) ) ;
#3135 = VERTEX_POINT ( 'NONE', #17304 ) ;
#3136 = CARTESIAN_POINT ( 'NONE',  ( -4.000000000000000000, 0.8576368993457507139, -3.433240632782198709 ) ) ;
#3137 = EDGE_CURVE ( 'NONE', #11692, #6003, #13869, .T. ) ;
#3138 = CIRCLE ( 'NONE', #12566, 23.50000000000001066 ) ;
#3139 = CARTESIAN_POINT ( 'NONE',  ( 2.345747346278113987, -3.264484291692503870, -0.01223254789874484924 ) ) ;
#3140 = DIRECTION ( 'NONE',  ( 0.000000000000000000, -0.9510565162951565288, 0.3090169943749383474 ) ) ;
#3141 = CARTESIAN_POINT ( 'NONE',  ( 0.000000000000000000, 45.00825343885067298, -33.95787273855199828 ) ) ;
#3142 = ORIENTED_EDGE ( 'NONE', *, *, #6093, .T. ) ;
#3143 = CLOSED_SHELL ( 'NONE', ( #5760, #17055, #1217, #6071, #8539, #14895, #11698, #13435, #3863, #14257, #17180, #2730, #4030, #5733, #6866, #6096, #17687, #8203, #7082, #14045, #6805, #3650, #6257, #5881, #5285, #4348, #10440, #14230, #16768, #10129, #13340, #11631, #4025, #10069, #9467, #2834, #1095 ) ) ;
#3144 = DIRECTION ( 'NONE',  ( 0.000000000000000000, -0.000000000000000000, -1.000000000000000000 ) ) ;
#3145 = FACE_OUTER_BOUND ( 'NONE', #18317, .T. ) ;
#3146 = VERTEX_POINT ( 'NONE', #9768 ) ;
#3147 = CARTESIAN_POINT ( 'NONE',  ( 0.000000000000000000, 19.44239304137403579, -20.41355805489595454 ) ) ;
#3148 = DIRECTION ( 'NONE',  ( 1.000000000000000000, 0.000000000000000000, 0.000000000000000000 ) ) ;
#3149 = AXIS2_PLACEMENT_3D ( 'NONE', #3748, #9750, #9547 ) ;
#3150 = ORIENTED_EDGE ( 'NONE', *, *, #7870, .T. ) ;
#3151 = CARTESIAN_POINT ( 'NONE',  ( -11.15000000000000391, 0.000000000000000000, 0.000000000000000000 ) ) ;
#3152 = CARTESIAN_POINT ( 'NONE',  ( 10.00000000000000000, -16.10733642026522006, 53.89344778774807310 ) ) ;
#3153 = ORIENTED_EDGE ( 'NONE', *, *, #2185, .T. ) ;
#3154 = CARTESIAN_POINT ( 'NONE',  ( -12.69999999999999929, 0.000000000000000000, -28.00000000000000355 ) ) ;
#3155 = DIRECTION ( 'NONE',  ( 0.000000000000000000, 0.000000000000000000, 1.000000000000000000 ) ) ;
#3156 = DIRECTION ( 'NONE',  ( -0.000000000000000000, 1.000000000000000000, -0.000000000000000000 ) ) ;
#3157 = CARTESIAN_POINT ( 'NONE',  ( -1.250000000000000000, -6.429618962271402616, 0.000000000000000000 ) ) ;
#3158 = VERTEX_POINT ( 'NONE', #2811 ) ;
#3159 = DIRECTION ( 'NONE',  ( 1.000000000000000000, 0.000000000000000000, 0.000000000000000000 ) ) ;
#3160 = VERTEX_POINT ( 'NONE', #14516 ) ;
#3161 =( GEOMETRIC_REPRESENTATION_CONTEXT ( 3 ) GLOBAL_UNCERTAINTY_ASSIGNED_CONTEXT ( ( #15290 ) ) GLOBAL_UNIT_ASSIGNED_CONTEXT ( ( #14683, #18007, #11919 ) ) REPRESENTATION_CONTEXT ( 'NONE', 'WORKASPACE' ) );
#3162 = FILL_AREA_STYLE_COLOUR ( '', #1350 ) ;
#3163 = CARTESIAN_POINT ( 'NONE',  ( 12.49999999999999289, 3.306546357697853733E-15, 27.00000000000000000 ) ) ;
#3164 = ORIENTED_EDGE ( 'NONE', *, *, #9412, .F. ) ;
#3165 = ORIENTED_EDGE ( 'NONE', *, *, #10662, .T. ) ;
#3166 = EDGE_CURVE ( 'NONE', #4962, #11121, #8096, .T. ) ;
#3167 = ADVANCED_FACE ( 'NONE', ( #8617 ), #14144, .T. ) ;
#3168 = ORIENTED_EDGE ( 'NONE', *, *, #16807, .F. ) ;
#3169 = VERTEX_POINT ( 'NONE', #15578 ) ;
#3170 =( GEOMETRIC_REPRESENTATION_CONTEXT ( 3 ) GLOBAL_UNCERTAINTY_ASSIGNED_CONTEXT ( ( #17765 ) ) GLOBAL_UNIT_ASSIGNED_CONTEXT ( ( #7673, #10718, #736 ) ) REPRESENTATION_CONTEXT ( 'NONE', 'WORKASPACE' ) );
#3171 = DIRECTION ( 'NONE',  ( 0.000000000000000000, 0.5877852522924686962, 0.8090169943749507819 ) ) ;
#3172 = EDGE_CURVE ( 'NONE', #5933, #17054, #16009, .T. ) ;
#3173 = DIRECTION ( 'NONE',  ( 1.000000000000000000, 0.000000000000000000, 0.000000000000000000 ) ) ;
#3174 = DIRECTION ( 'NONE',  ( 0.000000000000000000, 0.000000000000000000, 1.000000000000000000 ) ) ;
#3175 = CARTESIAN_POINT ( 'NONE',  ( -56.50000000009000445, -30.00000000000000000, 3.817814120399276590E-13 ) ) ;
#3176 = ADVANCED_FACE ( 'NONE', ( #4254 ), #15863, .T. ) ;
#3177 = LINE ( 'NONE', #8356, #12393 ) ;
#3178 = FACE_BOUND ( 'NONE', #15130, .T. ) ;
#3179 = DIRECTION ( 'NONE',  ( -1.000000000000000000, -0.000000000000000000, 0.000000000000000000 ) ) ;
#3180 = DIRECTION ( 'NONE',  ( -1.000000000000000000, -0.000000000000000000, -0.000000000000000000 ) ) ;
#3181 = ORIENTED_EDGE ( 'NONE', *, *, #7944, .T. ) ;
#3182 = FACE_OUTER_BOUND ( 'NONE', #12508, .T. ) ;
#3183 = EDGE_CURVE ( 'NONE', #6177, #10381, #12970, .T. ) ;
#3184 = CARTESIAN_POINT ( 'NONE',  ( 10.00000000000000000, -49.76630880786289879, -26.49895292618059273 ) ) ;
#3185 = CARTESIAN_POINT ( 'NONE',  ( 0.000000000000000000, -17.25000000000000355, 0.000000000000000000 ) ) ;
#3186 = VERTEX_POINT ( 'NONE', #6908 ) ;
#3187 = ORIENTED_EDGE ( 'NONE', *, *, #10546, .F. ) ;
#3188 =( REPRESENTATION_RELATIONSHIP ('NONE','NONE', #11014, #2517 ) REPRESENTATION_RELATIONSHIP_WITH_TRANSFORMATION ( #16978 )SHAPE_REPRESENTATION_RELATIONSHIP( ) );
#3189 = LINE ( 'NONE', #13287, #9606 ) ;
#3190 = DIRECTION ( 'NONE',  ( 6.123233995736766036E-17, -1.000000000000000000, 0.000000000000000000 ) ) ;
#3191 = AXIS2_PLACEMENT_3D ( 'NONE', #4703, #6136, #17851 ) ;
#3192 = CARTESIAN_POINT ( 'NONE',  ( 10.00000000000000000, -53.22058882792220658, 33.71303790549256263 ) ) ;
#3193 = VERTEX_POINT ( 'NONE', #1207 ) ;
#3194 = VECTOR ( 'NONE', #17698, 1000.000000000000000 ) ;
#3195 = ADVANCED_FACE ( 'NONE', ( #5849 ), #12038, .F. ) ;
#3196 = EDGE_CURVE ( 'NONE', #6730, #16191, #18534, .T. ) ;
#3197 = CARTESIAN_POINT ( 'NONE',  ( -117.1020693116506379, -30.00000000000000000, -22.34080595179799644 ) ) ;
#3198 = EDGE_CURVE ( 'NONE', #16109, #6670, #4429, .T. ) ;
#3199 = FACE_OUTER_BOUND ( 'NONE', #18198, .T. ) ;
#3200 = CARTESIAN_POINT ( 'NONE',  ( 10.00000000000000000, -53.92768374110902840, 16.45250512421837641 ) ) ;
#3201 = ADVANCED_FACE ( 'NONE', ( #9859 ), #14337, .T. ) ;
#3202 = ORIENTED_EDGE ( 'NONE', *, *, #17282, .T. ) ;
#3203 = DIRECTION ( 'NONE',  ( -1.000000000000000000, -0.000000000000000000, 0.000000000000000000 ) ) ;
#3204 = CIRCLE ( 'NONE', #8668, 26.24900000002624978 ) ;
#3205 = VERTEX_POINT ( 'NONE', #12820 ) ;
#3206 = DIRECTION ( 'NONE',  ( 0.000000000000000000, 0.3090169943749479509, -0.9510565162951533091 ) ) ;
#3207 = CIRCLE ( 'NONE', #8063, 5.000000000000000000 ) ;
#3208 = ORIENTED_EDGE ( 'NONE', *, *, #10834, .T. ) ;
#3209 = DIRECTION ( 'NONE',  ( 1.000000000000000000, 0.000000000000000000, 0.000000000000000000 ) ) ;
#3210 = FACE_OUTER_BOUND ( 'NONE', #1680, .T. ) ;
#3211 = ORIENTED_EDGE ( 'NONE', *, *, #11591, .T. ) ;
#3212 = ORIENTED_EDGE ( 'NONE', *, *, #896, .T. ) ;
#3213 = LINE ( 'NONE', #9010, #2910 ) ;
#3214 = ORIENTED_EDGE ( 'NONE', *, *, #8068, .T. ) ;
#3215 = CARTESIAN_POINT ( 'NONE',  ( 10.00000000000000000, -25.38428207620317778, -6.681932690257235130 ) ) ;
#3216 = AXIS2_PLACEMENT_3D ( 'NONE', #15972, #12849, #5703 ) ;
#3217 = AXIS2_PLACEMENT_3D ( 'NONE', #10704, #6234, #14814 ) ;
#3218 = VECTOR ( 'NONE', #2004, 1000.000000000000000 ) ;
#3219 = DIRECTION ( 'NONE',  ( 0.000000000000000000, -1.000000000000000000, -1.047444401652940164E-14 ) ) ;
#3220 = EDGE_CURVE ( 'NONE', #17928, #1108, #18438, .T. ) ;
#3221 = VERTEX_POINT ( 'NONE', #9957 ) ;
#3222 = ORIENTED_EDGE ( 'NONE', *, *, #2827, .T. ) ;
#3223 = DIRECTION ( 'NONE',  ( 0.000000000000000000, 0.000000000000000000, 1.000000000000000000 ) ) ;
#3224 = DIRECTION ( 'NONE',  ( 0.000000000000000000, 0.000000000000000000, 1.000000000000000000 ) ) ;
#3226 = AXIS2_PLACEMENT_3D ( 'NONE', #6860, #4018, #9819 ) ;
#3225 = DIRECTION ( 'NONE',  ( 0.000000000000000000, 0.000000000000000000, 1.000000000000000000 ) ) ;
#3227 = EDGE_LOOP ( 'NONE', ( #14533, #10465 ) ) ;
#3228 = CARTESIAN_POINT ( 'NONE',  ( -90.00000000009003998, 1.000000000000018208, -5.746271514173173500E-15 ) ) ;
#3229 = VECTOR ( 'NONE', #18217, 999.9999999999998863 ) ;
#3230 = DIRECTION ( 'NONE',  ( 0.000000000000000000, 0.000000000000000000, 1.000000000000000000 ) ) ;
#3231 = DIRECTION ( 'NONE',  ( -0.000000000000000000, -0.000000000000000000, -1.000000000000000000 ) ) ;
#3232 = AXIS2_PLACEMENT_3D ( 'NONE', #12714, #4988, #9378 ) ;
#3233 = FACE_BOUND ( 'NONE', #18034, .T. ) ;
#3234 = VERTEX_POINT ( 'NONE', #15773 ) ;
#3235 = CARTESIAN_POINT ( 'NONE',  ( 0.000000000000000000, -13.40641754777683126, 24.79895094899255170 ) ) ;
#3236 = AXIS2_PLACEMENT_3D ( 'NONE', #17111, #13547, #11484 ) ;
#3237 = ORIENTED_EDGE ( 'NONE', *, *, #518, .T. ) ;
#3238 = PLANE ( 'NONE',  #17315 ) ;
#3239 = DIRECTION ( 'NONE',  ( -1.000000000000000000, 0.000000000000000000, -0.000000000000000000 ) ) ;
#3240=STYLED_ITEM('',(#18876),#3564);
#3241 = EDGE_CURVE ( 'NONE', #16413, #16577, #5359, .T. ) ;
#3242 = AXIS2_PLACEMENT_3D ( 'NONE', #8015, #12119, #13555 ) ;
#3243 = MANIFOLD_SOLID_BREP ( 'RollersSimplified', #1327 ) ;
#3244 = AXIS2_PLACEMENT_3D ( 'NONE', #2382, #6575, #12381 ) ;
#3245 = ORIENTED_EDGE ( 'NONE', *, *, #14824, .F. ) ;
#3246 = FACE_OUTER_BOUND ( 'NONE', #13686, .T. ) ;
#3247 = DIRECTION ( 'NONE',  ( 0.000000000000000000, 0.000000000000000000, 1.000000000000000000 ) ) ;
#3248 = ORIENTED_EDGE ( 'NONE', *, *, #4834, .T. ) ;
#3249 = DIRECTION ( 'NONE',  ( -1.000000000000000000, -0.000000000000000000, -0.000000000000000000 ) ) ;
#3250 = FACE_OUTER_BOUND ( 'NONE', #18743, .T. ) ;
#3251 = DIRECTION ( 'NONE',  ( -0.000000000000000000, 1.000000000000000000, -0.000000000000000000 ) ) ;
#3252 = CIRCLE ( 'NONE', #8425, 24.00000000002399858 ) ;
#3253 = CARTESIAN_POINT ( 'NONE',  ( 1.250000000000000000, -6.429618962271402616, 0.000000000000000000 ) ) ;
#3254 = ORIENTED_EDGE ( 'NONE', *, *, #7254, .F. ) ;
#3255 = DIRECTION ( 'NONE',  ( -1.000000000000000000, -0.000000000000000000, 0.000000000000000000 ) ) ;
#3256 = ORIENTED_EDGE ( 'NONE', *, *, #13395, .T. ) ;
#3257 = CIRCLE ( 'NONE', #14206, 12.00000000001200462 ) ;
#3258 = DIRECTION ( 'NONE',  ( 0.000000000000000000, 0.000000000000000000, 1.000000000000000000 ) ) ;
#3259 = ORIENTED_EDGE ( 'NONE', *, *, #15306, .T. ) ;
#3260 = AXIS2_PLACEMENT_3D ( 'NONE', #16931, #3880, #1495 ) ;
#3261 = AXIS2_PLACEMENT_3D ( 'NONE', #15688, #2640, #7023 ) ;
#3262 = EDGE_CURVE ( 'NONE', #3665, #8441, #14904, .T. ) ;
#3263 = ORIENTED_EDGE ( 'NONE', *, *, #17390, .T. ) ;
#3264 = EDGE_CURVE ( 'NONE', #15594, #13366, #11740, .T. ) ;
#3265 = ORIENTED_EDGE ( 'NONE', *, *, #7721, .F. ) ;
#3266 = AXIS2_PLACEMENT_3D ( 'NONE', #10092, #8654, #16991 ) ;
#3267 = ORIENTED_EDGE ( 'NONE', *, *, #14108, .T. ) ;
#3268 = CIRCLE ( 'NONE', #4774, 33.00000000003299760 ) ;
#3269 = FACE_OUTER_BOUND ( 'NONE', #6748, .T. ) ;
#3270 = CARTESIAN_POINT ( 'NONE',  ( -87.43997332177200121, -10.00000000000001954, 6.475821446449876007 ) ) ;
#3271 = VECTOR ( 'NONE', #2914, 1000.000000000000000 ) ;
#3272 = AXIS2_PLACEMENT_3D ( 'NONE', #11356, #14219, #9744 ) ;
#3273 = FACE_OUTER_BOUND ( 'NONE', #7411, .T. ) ;
#3274 = DIRECTION ( 'NONE',  ( -1.000000000000000000, -0.000000000000000000, -0.000000000000000000 ) ) ;
#3275 = FACE_OUTER_BOUND ( 'NONE', #10621, .T. ) ;
#3276 = FACE_OUTER_BOUND ( 'NONE', #6379, .T. ) ;
#3277 = DIRECTION ( 'NONE',  ( 0.000000000000000000, 0.000000000000000000, 1.000000000000000000 ) ) ;
#3278 = DIRECTION ( 'NONE',  ( -1.000000000000000000, -0.000000000000000000, -0.000000000000000000 ) ) ;
#3279 = ORIENTED_EDGE ( 'NONE', *, *, #11591, .F. ) ;
#3280 = EDGE_CURVE ( 'NONE', #1091, #16517, #16323, .T. ) ;
#3281 = CARTESIAN_POINT ( 'NONE',  ( 10.00000000000000000, -3.730438010304114371, -27.94286728106396822 ) ) ;
#3282 = DIRECTION ( 'NONE',  ( 0.000000000000000000, 0.000000000000000000, 1.000000000000000000 ) ) ;
#3283 = FACE_OUTER_BOUND ( 'NONE', #15647, .T. ) ;
#3284 = ORIENTED_EDGE ( 'NONE', *, *, #9923, .T. ) ;
#3285 = VERTEX_POINT ( 'NONE', #3007 ) ;
#3286 = CARTESIAN_POINT ( 'NONE',  ( -36.40576474687247099, 10.00000000000000000, 26.45033635316149301 ) ) ;
#3287 = DIRECTION ( 'NONE',  ( 0.000000000000000000, 0.000000000000000000, 1.000000000000000000 ) ) ;
#3288 = PRODUCT_RELATED_PRODUCT_CATEGORY ( 'part', '', ( #9804 ) ) ;
#3289 = LINE ( 'NONE', #17576, #5759 ) ;
#3290 = ORIENTED_EDGE ( 'NONE', *, *, #16108, .F. ) ;
#3291 = CIRCLE ( 'NONE', #7242, 26.24900000002624978 ) ;
#3292 = AXIS2_PLACEMENT_3D ( 'NONE', #794, #18505, #6600 ) ;
#3293 = PRODUCT ( 'base plate', 'base plate', '', ( #2705 ) ) ;
#3294 = DIRECTION ( 'NONE',  ( 0.000000000000000000, 0.000000000000000000, -1.000000000000000000 ) ) ;
#3295 = CARTESIAN_POINT ( 'NONE',  ( 0.000000000000000000, 3.730438010304726770, -27.94286728106388296 ) ) ;
#3296 = CIRCLE ( 'NONE', #4214, 26.24900000002625333 ) ;
#3297 = CARTESIAN_POINT ( 'NONE',  ( 5.000000000000000000, 61.03368945066435458, 15.61693798565518065 ) ) ;
#3298 = ORIENTED_EDGE ( 'NONE', *, *, #18213, .T. ) ;
#3299 = CARTESIAN_POINT ( 'NONE',  ( 2.344047193898588954, 3.265465875126468021, -5.031375706690542042E-16 ) ) ;
#3300 = AXIS2_PLACEMENT_3D ( 'NONE', #217, #7541, #4679 ) ;
#3301 = CIRCLE ( 'NONE', #2389, 33.00000000003299760 ) ;
#3302 = EDGE_LOOP ( 'NONE', ( #13752, #17572 ) ) ;
#3303 = CIRCLE ( 'NONE', #14539, 4.250000000000000000 ) ;
#3304 = DIRECTION ( 'NONE',  ( -1.000000000000000000, 0.000000000000000000, 0.000000000000000000 ) ) ;
#3305 = VERTEX_POINT ( 'NONE', #17470 ) ;
#3306 =( REPRESENTATION_RELATIONSHIP ('NONE','NONE', #11014, #16132 ) REPRESENTATION_RELATIONSHIP_WITH_TRANSFORMATION ( #5653 )SHAPE_REPRESENTATION_RELATIONSHIP( ) );
#3307 = EDGE_CURVE ( 'NONE', #12824, #6434, #3096, .T. ) ;
#3308 = ADVANCED_FACE ( 'NONE', ( #1570 ), #1407, .T. ) ;
#3309 = EDGE_CURVE ( 'NONE', #9576, #3525, #10215, .T. ) ;
#3310 = EDGE_CURVE ( 'NONE', #6304, #3994, #142, .T. ) ;
#3311 = CARTESIAN_POINT ( 'NONE',  ( -90.00000000009001155, -13.00000000000001776, -1.301042606982603940E-15 ) ) ;
#3312 = CYLINDRICAL_SURFACE ( 'NONE', #3435, 63.00000000006298961 ) ;
#3313 = ORIENTED_EDGE ( 'NONE', *, *, #9224, .T. ) ;
#3314 = ORIENTED_EDGE ( 'NONE', *, *, #8076, .F. ) ;
#3315 = DIRECTION ( 'NONE',  ( -1.000000000000000000, -0.000000000000000000, 0.000000000000000000 ) ) ;
#3316 =( LENGTH_UNIT ( ) NAMED_UNIT ( * ) SI_UNIT ( .MILLI., .METRE. ) );
#3317 = ADVANCED_FACE ( 'NONE', ( #10233 ), #12025, .T. ) ;
#3318 = ORIENTED_EDGE ( 'NONE', *, *, #5395, .T. ) ;
#3319 = DIRECTION ( 'NONE',  ( 0.000000000000000000, 0.000000000000000000, 1.000000000000000000 ) ) ;
#3320 = AXIS2_PLACEMENT_3D ( 'NONE', #12306, #11167, #13832 ) ;
#3321 = VECTOR ( 'NONE', #10379, 1000.000000000000000 ) ;
#3322 = AXIS2_PLACEMENT_3D ( 'NONE', #10512, #16332, #149 ) ;
#3323 = CIRCLE ( 'NONE', #8189, 12.00000000001200284 ) ;
#3324 = CIRCLE ( 'NONE', #5448, 56.24900000005626310 ) ;
#3325 = EDGE_CURVE ( 'NONE', #10104, #7022, #12343, .T. ) ;
#3326 = CARTESIAN_POINT ( 'NONE',  ( 10.00000000000000000, 0.000000000000000000, 0.000000000000000000 ) ) ;
#3327 = EDGE_LOOP ( 'NONE', ( #1416, #15430, #9342, #5545 ) ) ;
#3328 = AXIS2_PLACEMENT_3D ( 'NONE', #18509, #5470, #11360 ) ;
#3329 = ORIENTED_EDGE ( 'NONE', *, *, #11324, .F. ) ;
#3330 = DIRECTION ( 'NONE',  ( 1.000000000000000000, 0.000000000000000000, 0.000000000000000000 ) ) ;
#3331 = DIRECTION ( 'NONE',  ( 0.000000000000000000, 0.000000000000000000, 1.000000000000000000 ) ) ;
#3332 = CARTESIAN_POINT ( 'NONE',  ( 10.00000000000000000, -26.49895292617967257, -49.76630880786338196 ) ) ;
#3333 = VERTEX_POINT ( 'NONE', #6038 ) ;
#3334 = CARTESIAN_POINT ( 'NONE',  ( 2.691179338796023329E-15, 4.647089433458991614, -3.572167766733753691 ) ) ;
#3335 = ADVANCED_FACE ( 'NONE', ( #3182 ), #11851, .T. ) ;
#3336 = AXIS2_PLACEMENT_3D ( 'NONE', #14368, #7116, #7217 ) ;
#3337 = DIRECTION ( 'NONE',  ( -1.000000000000000000, 0.000000000000000000, -0.000000000000000000 ) ) ;
#3338 = DIRECTION ( 'NONE',  ( 0.000000000000000000, 0.000000000000000000, -1.000000000000000000 ) ) ;
#3339 = DIRECTION ( 'NONE',  ( 0.000000000000000000, 0.000000000000000000, 1.000000000000000000 ) ) ;
#3340 = ORIENTED_EDGE ( 'NONE', *, *, #5855, .F. ) ;
#3341 = DIRECTION ( 'NONE',  ( 0.000000000000000000, 0.000000000000000000, -1.000000000000000000 ) ) ;
#3342 = CARTESIAN_POINT ( 'NONE',  ( 10.00000000000000000, -27.94286728106395756, 3.730438010304225394 ) ) ;
#3343 = ORIENTED_EDGE ( 'NONE', *, *, #1461, .F. ) ;
#3344 = CARTESIAN_POINT ( 'NONE',  ( 0.000000000000000000, 61.03368945066435458, 15.61693798565518421 ) ) ;
#3345 = CARTESIAN_POINT ( 'NONE',  ( 32.50000000000000000, -26.50000000000000000, 2.650000000000367617 ) ) ;
#3346 = EDGE_CURVE ( 'NONE', #4781, #17733, #5031, .T. ) ;
#3347 = AXIS2_PLACEMENT_3D ( 'NONE', #5723, #2570, #15537 ) ;
#3348 = CIRCLE ( 'NONE', #297, 4.799999999999998934 ) ;
#3349 = ORIENTED_EDGE ( 'NONE', *, *, #7624, .T. ) ;
#3350 = DIRECTION ( 'NONE',  ( 0.000000000000000000, -0.4999999999999992228, 0.8660254037844390407 ) ) ;
#3351 = ORIENTED_EDGE ( 'NONE', *, *, #12168, .T. ) ;
#3352 = CARTESIAN_POINT ( 'NONE',  ( 0.000000000000000000, -53.92768374110902840, 16.45250512421837641 ) ) ;
#3353 = DIRECTION ( 'NONE',  ( 0.000000000000000000, 0.000000000000000000, 1.000000000000000000 ) ) ;
#3354 = CARTESIAN_POINT ( 'NONE',  ( 45.00000000000000000, 0.000000000000000000, 2.649999999999487432 ) ) ;
#3355 = CARTESIAN_POINT ( 'NONE',  ( 5.000000000000000000, 41.62350880771921169, 47.29147401531970019 ) ) ;
#3356 = ORIENTED_EDGE ( 'NONE', *, *, #6693, .T. ) ;
#3357 = CARTESIAN_POINT ( 'NONE',  ( 1.250000000000000000, -6.429618962271402616, -1.000000000000000000 ) ) ;
#3358 = ORIENTED_EDGE ( 'NONE', *, *, #7325, .T. ) ;
#3359 = DIRECTION ( 'NONE',  ( 0.000000000000000000, -0.5877852522924622569, -0.8090169943749552228 ) ) ;
#3360 = VERTEX_POINT ( 'NONE', #14799 ) ;
#3361 = ADVANCED_FACE ( 'NONE', ( #1749 ), #13384, .T. ) ;
#3362 = ORIENTED_EDGE ( 'NONE', *, *, #11569, .F. ) ;
#3363 = ORIENTED_EDGE ( 'NONE', *, *, #4070, .F. ) ;
#3364 = ORIENTED_EDGE ( 'NONE', *, *, #5872, .T. ) ;
#3365 = AXIS2_PLACEMENT_3D ( 'NONE', #2298, #18684, #12886 ) ;
#3366 = PLANE ( 'NONE',  #9913 ) ;
#3367 = CARTESIAN_POINT ( 'NONE',  ( 10.00000000000000000, -24.68609584167194981, 50.69000562871634230 ) ) ;
#3368 = EDGE_CURVE ( 'NONE', #6276, #8847, #8392, .T. ) ;
#3369 = DIRECTION ( 'NONE',  ( 0.000000000000000000, 0.000000000000000000, 1.000000000000000000 ) ) ;
#3370 = CARTESIAN_POINT ( 'NONE',  ( 5.000000000000000000, -41.62350880771888484, -47.29147401531999861 ) ) ;
#3371 = DIRECTION ( 'NONE',  ( -1.000000000000000000, 0.000000000000000000, -0.000000000000000000 ) ) ;
#3372 = CARTESIAN_POINT ( 'NONE',  ( 4.000000000000000000, 2.309401076758497151, -3.433295621305379353 ) ) ;
#3373 = ORIENTED_EDGE ( 'NONE', *, *, #5819, .F. ) ;
#3374 = FACE_OUTER_BOUND ( 'NONE', #8792, .T. ) ;
#3375 = EDGE_LOOP ( 'NONE', ( #6819, #11602, #8987, #13775 ) ) ;
#3376 = EDGE_CURVE ( 'NONE', #12396, #16921, #15699, .T. ) ;
#3377 = CARTESIAN_POINT ( 'NONE',  ( -4.078421086530219064, -3.990950201428956845, -1.000000000000000000 ) ) ;
#3378 = CYLINDRICAL_SURFACE ( 'NONE', #9842, 12.00000000001200640 ) ;
#3379 = DIRECTION ( 'NONE',  ( 0.000000000000000000, 0.000000000000000000, 1.000000000000000000 ) ) ;
#3380 = ORIENTED_EDGE ( 'NONE', *, *, #7272, .T. ) ;
#3381 = ORIENTED_EDGE ( 'NONE', *, *, #7118, .F. ) ;
#3382 = DIRECTION ( 'NONE',  ( 0.000000000000000000, 0.000000000000000000, -1.000000000000000000 ) ) ;
#3383 = AXIS2_PLACEMENT_3D ( 'NONE', #8267, #942, #18351 ) ;
#3384 = DIRECTION ( 'NONE',  ( 0.000000000000000000, 0.000000000000000000, 1.000000000000000000 ) ) ;
#3385 = DIRECTION ( 'NONE',  ( -0.000000000000000000, 1.000000000000000000, 0.000000000000000000 ) ) ;
#3386 = EDGE_LOOP ( 'NONE', ( #16072, #1648, #4851, #3697 ) ) ;
#3387 = LINE ( 'NONE', #532, #4141 ) ;
#3388 = CYLINDRICAL_SURFACE ( 'NONE', #15829, 2.649999999999999467 ) ;
#3389 = CARTESIAN_POINT ( 'NONE',  ( 5.000000000000000000, 29.75305054077472633, 14.27431201565535979 ) ) ;
#3390 = EDGE_LOOP ( 'NONE', ( #128, #14960, #7663, #3037 ) ) ;
#3392 = AXIS2_PLACEMENT_3D ( 'NONE', #4713, #347, #13400 ) ;
#3391 = CARTESIAN_POINT ( 'NONE',  ( 1.655952806101427033, -3.662737355149048302, -1.182683869819604841E-14 ) ) ;
#3393 = VERTEX_POINT ( 'NONE', #8489 ) ;
#3394 = DIRECTION ( 'NONE',  ( -0.000000000000000000, 1.000000000000000000, -0.000000000000000000 ) ) ;
#3395 = ORIENTED_EDGE ( 'NONE', *, *, #5622, .T. ) ;
#3396 = CIRCLE ( 'NONE', #1286, 2.649999999999999467 ) ;
#3397 = FACE_OUTER_BOUND ( 'NONE', #1918, .T. ) ;
#3398 = CIRCLE ( 'NONE', #16480, 27.00000000000000355 ) ;
#3399 = CARTESIAN_POINT ( 'NONE',  ( 2.500000000000000444, 0.000000000000000000, -5.000000000000000888 ) ) ;
#3400 = ORIENTED_EDGE ( 'NONE', *, *, #681, .F. ) ;
#3401 = ORIENTED_EDGE ( 'NONE', *, *, #12, .F. ) ;
#3402 = DIRECTION ( 'NONE',  ( -0.000000000000000000, 1.000000000000000000, -0.000000000000000000 ) ) ;
#3403 =( NAMED_UNIT ( * ) PLANE_ANGLE_UNIT ( ) SI_UNIT ( $, .RADIAN. ) );
#3404 = ORIENTED_EDGE ( 'NONE', *, *, #17059, .T. ) ;
#3405 = FACE_OUTER_BOUND ( 'NONE', #2624, .T. ) ;
#3406 = AXIS2_PLACEMENT_3D ( 'NONE', #5082, #4984, #11071 ) ;
#3407 = EDGE_CURVE ( 'NONE', #17793, #14080, #4739, .T. ) ;
#3408 = EDGE_CURVE ( 'NONE', #13093, #125, #1101, .T. ) ;
#3409 = AXIS2_PLACEMENT_3D ( 'NONE', #14852, #11536, #17429 ) ;
#3410 = FACE_OUTER_BOUND ( 'NONE', #13392, .T. ) ;
#3411 = ADVANCED_FACE ( 'NONE', ( #11250 ), #15443, .T. ) ;
#3412 = EDGE_LOOP ( 'NONE', ( #17004, #11269, #15266, #16917, #10570, #17081, #11839, #550, #6207, #11325, #994, #93 ) ) ;
#3413 = ADVANCED_FACE ( 'NONE', ( #14099 ), #1060, .T. ) ;
#3414 = VERTEX_POINT ( 'NONE', #14013 ) ;
#3415 = CYLINDRICAL_SURFACE ( 'NONE', #15730, 2.649999999999992806 ) ;
#3416 = DIRECTION ( 'NONE',  ( -0.01515971714484241201, 0.000000000000000000, 0.9998850848853023665 ) ) ;
#3417 = CARTESIAN_POINT ( 'NONE',  ( 0.000000000000000000, 0.5192545390863916310, -1.000000000000000000 ) ) ;
#3418 = ORIENTED_EDGE ( 'NONE', *, *, #2007, .F. ) ;
#3419 = CARTESIAN_POINT ( 'NONE',  ( -90.00000000009001155, -49.14213562373095812, -5.000000000000005329 ) ) ;
#3420 = EDGE_CURVE ( 'NONE', #514, #16495, #6969, .T. ) ;
#3421 = DIRECTION ( 'NONE',  ( 0.000000000000000000, 0.000000000000000000, 1.000000000000000000 ) ) ;
#3422 = FACE_BOUND ( 'NONE', #14128, .T. ) ;
#3423 = FACE_OUTER_BOUND ( 'NONE', #3682, .T. ) ;
#3424 = ORIENTED_EDGE ( 'NONE', *, *, #15143, .F. ) ;
#3425 = DIRECTION ( 'NONE',  ( 0.000000000000000000, 0.9510565162951523099, 0.3090169943749516701 ) ) ;
#3426 = CARTESIAN_POINT ( 'NONE',  ( 10.00000000000000000, -7.478235706489372525, 55.74967257055880054 ) ) ;
#3427 = AXIS2_PLACEMENT_3D ( 'NONE', #8658, #1699, #14 ) ;
#3429 = EDGE_CURVE ( 'NONE', #243, #18412, #12129, .T. ) ;
#3428 = ORIENTED_EDGE ( 'NONE', *, *, #5058, .F. ) ;
#3430 = DIRECTION ( 'NONE',  ( 0.000000000000000000, 0.000000000000000000, 1.000000000000000000 ) ) ;
#3431 = DIRECTION ( 'NONE',  ( 0.000000000000000000, 0.000000000000000000, -1.000000000000000000 ) ) ;
#3432 = ADVANCED_FACE ( 'NONE', ( #13663 ), #10694, .T. ) ;
#3433 = EDGE_CURVE ( 'NONE', #12463, #15108, #11438, .T. ) ;
#3434 = ORIENTED_EDGE ( 'NONE', *, *, #9228, .T. ) ;
#3435 = AXIS2_PLACEMENT_3D ( 'NONE', #13689, #18052, #10806 ) ;
#3436 = CARTESIAN_POINT ( 'NONE',  ( 10.00000000000000000, -25.42247726998023083, 12.18267823974742470 ) ) ;
#3437 = CIRCLE ( 'NONE', #9204, 26.24900000002625333 ) ;
#3438 = ORIENTED_EDGE ( 'NONE', *, *, #11471, .F. ) ;
#3439 = AXIS2_PLACEMENT_3D ( 'NONE', #7520, #17623, #16193 ) ;
#3440 = CARTESIAN_POINT ( 'NONE',  ( -3.264624719419710521E-13, -4.796980096169328966, -3.721999068284310486 ) ) ;
#3441 = EDGE_CURVE ( 'NONE', #9657, #14680, #6769, .T. ) ;
#3442 = DIRECTION ( 'NONE',  ( 0.000000000000000000, 0.000000000000000000, -1.000000000000000000 ) ) ;
#3443 = FACE_OUTER_BOUND ( 'NONE', #17179, .T. ) ;
#3444 = CYLINDRICAL_SURFACE ( 'NONE', #7956, 2.649999999999995914 ) ;
#3445 = CARTESIAN_POINT ( 'NONE',  ( -4.211140560182196957, -2.431303136016552013, -3.745885042887436178 ) ) ;
#3446 = ORIENTED_EDGE ( 'NONE', *, *, #12426, .T. ) ;
#3447 = DIRECTION ( 'NONE',  ( -1.000000000000000000, -0.000000000000000000, 0.000000000000000000 ) ) ;
#3448 = PRODUCT_DEFINITION_SHAPE ( 'NONE', 'NONE',  #18832 ) ;
#3449 =( NAMED_UNIT ( * ) SI_UNIT ( $, .STERADIAN. ) SOLID_ANGLE_UNIT ( ) );
#3450 = DIRECTION ( 'NONE',  ( -1.000000000000000000, -0.000000000000000000, -0.000000000000000000 ) ) ;
#3451 = ORIENTED_EDGE ( 'NONE', *, *, #4742, .F. ) ;
#3452 = CONTEXT_DEPENDENT_SHAPE_REPRESENTATION ( #13649, #7681 ) ;
#3453 = AXIS2_PLACEMENT_3D ( 'NONE', #13263, #10142, #15949 ) ;
#3454 = ORIENTED_EDGE ( 'NONE', *, *, #2712, .T. ) ;
#3455 = ORIENTED_EDGE ( 'NONE', *, *, #16189, .T. ) ;
#3456 = ORIENTED_EDGE ( 'NONE', *, *, #1827, .F. ) ;
#3457 = DIRECTION ( 'NONE',  ( -1.000000000000000000, -0.000000000000000000, 0.000000000000000000 ) ) ;
#3458 =( NAMED_UNIT ( * ) SI_UNIT ( $, .STERADIAN. ) SOLID_ANGLE_UNIT ( ) );
#3459 = CARTESIAN_POINT ( 'NONE',  ( 10.00000000000000000, -49.76630880786289879, -26.49895292618059273 ) ) ;
#3460 = EDGE_CURVE ( 'NONE', #1496, #7847, #2309, .T. ) ;
#3461 = DIRECTION ( 'NONE',  ( -0.000000000000000000, 1.000000000000000000, -0.000000000000000000 ) ) ;
#3462 = DIRECTION ( 'NONE',  ( -1.000000000000000000, 0.000000000000000000, 0.000000000000000000 ) ) ;
#3463 = PRESENTATION_LAYER_ASSIGNMENT (  '', '', ( #14113 ) ) ;
#3464 = DIRECTION ( 'NONE',  ( 1.000000000000000000, -0.000000000000000000, 0.000000000000000000 ) ) ;
#3465 = CYLINDRICAL_SURFACE ( 'NONE', #14086, 2.649999999999992806 ) ;
#3466 = DIRECTION ( 'NONE',  ( -1.000000000000000000, -0.000000000000000000, -0.000000000000000000 ) ) ;
#3467 = VERTEX_POINT ( 'NONE', #4977 ) ;
#3468 = DIRECTION ( 'NONE',  ( 0.000000000000000000, 0.000000000000000000, 1.000000000000000000 ) ) ;
#3469 = ORIENTED_EDGE ( 'NONE', *, *, #3325, .F. ) ;
#3470 = DIRECTION ( 'NONE',  ( -1.000000000000000000, 0.000000000000000000, 0.000000000000000000 ) ) ;
#3471 = FACE_OUTER_BOUND ( 'NONE', #10173, .T. ) ;
#3472 = CARTESIAN_POINT ( 'NONE',  ( 10.00000000000000000, -53.92768374110879392, -16.45250512421912603 ) ) ;
#3473 = ORIENTED_EDGE ( 'NONE', *, *, #17289, .F. ) ;
#3474 = ORIENTED_EDGE ( 'NONE', *, *, #10728, .T. ) ;
#3475 = CARTESIAN_POINT ( 'NONE',  ( 10.00000000000000000, 0.000000000000000000, 0.000000000000000000 ) ) ;
#3476 = CARTESIAN_POINT ( 'NONE',  ( 0.000000000000000000, 0.000000000000000000, 0.000000000000000000 ) ) ;
#3477 = CARTESIAN_POINT ( 'NONE',  ( 10.00000000000000000, 0.000000000000000000, 0.000000000000000000 ) ) ;
#3478 = ORIENTED_EDGE ( 'NONE', *, *, #8812, .T. ) ;
#3479 = EDGE_CURVE ( 'NONE', #2331, #7064, #14303, .T. ) ;
#3480 = EDGE_CURVE ( 'NONE', #3687, #5915, #7800, .T. ) ;
#3481 = DIRECTION ( 'NONE',  ( 0.000000000000000000, 0.000000000000000000, -1.000000000000000000 ) ) ;
#3482 = CARTESIAN_POINT ( 'NONE',  ( 4.211140560182196957, -2.431303136016555122, -3.745885042887436622 ) ) ;
#3483 = CYLINDRICAL_SURFACE ( 'NONE', #8141, 2.649999999999999467 ) ;
#3484 = ORIENTED_EDGE ( 'NONE', *, *, #16364, .T. ) ;
#3485 = CARTESIAN_POINT ( 'NONE',  ( 23.50000000000000355, 0.000000000000000000, -2.000000000000000000 ) ) ;
#3486 = VERTEX_POINT ( 'NONE', #5541 ) ;
#3487 = PLANE ( 'NONE',  #13336 ) ;
#3488 = VERTEX_POINT ( 'NONE', #16971 ) ;
#3489 = MECHANICAL_DESIGN_GEOMETRIC_PRESENTATION_REPRESENTATION (  '', ( #438 ), #10171 ) ;
#3490 = CARTESIAN_POINT ( 'NONE',  ( -90.00000000009001155, -29.99899999999999878, -1.301042606982605321E-15 ) ) ;
#3491 = CYLINDRICAL_SURFACE ( 'NONE', #2218, 63.00000000006298961 ) ;
#3492 = VERTEX_POINT ( 'NONE', #16603 ) ;
#3493 = EDGE_LOOP ( 'NONE', ( #2149, #2132, #10195, #7456 ) ) ;
#3494 = AXIS2_PLACEMENT_3D ( 'NONE', #9807, #17150, #13049 ) ;
#3495 = LINE ( 'NONE', #16451, #10796 ) ;
#3496 = VERTEX_POINT ( 'NONE', #18587 ) ;
#3497 = DIRECTION ( 'NONE',  ( -0.000000000000000000, 0.8660254037844391517, 0.4999999999999991673 ) ) ;
#3498 = EDGE_CURVE ( 'NONE', #15207, #34, #2011, .T. ) ;
#3499 = CARTESIAN_POINT ( 'NONE',  ( 2.712762565639649015, -3.052587955997662306, -3.430618716626630871 ) ) ;
#3500 = VECTOR ( 'NONE', #16543, 1000.000000000000000 ) ;
#3501 = CIRCLE ( 'NONE', #4120, 55.00000000000000000 ) ;
#3502 = ORIENTED_EDGE ( 'NONE', *, *, #4839, .T. ) ;
#3503 = ORIENTED_EDGE ( 'NONE', *, *, #14588, .T. ) ;
#3504 = DIRECTION ( 'NONE',  ( 0.000000000000000000, 1.000000000000000000, 0.000000000000000000 ) ) ;
#3505 = DIRECTION ( 'NONE',  ( 0.000000000000000000, 0.8090169943749444537, 0.5877852522924772449 ) ) ;
#3506 = CARTESIAN_POINT ( 'NONE',  ( 0.000000000000000000, 0.000000000000000000, 0.000000000000000000 ) ) ;
#3507 = EDGE_LOOP ( 'NONE', ( #14888, #591, #4877, #1000 ) ) ;
#3508 = LINE ( 'NONE', #17893, #3874 ) ;
#3509 = DIRECTION ( 'NONE',  ( -0.000000000000000000, 1.000000000000000000, -0.000000000000000000 ) ) ;
#3510 = CARTESIAN_POINT ( 'NONE',  ( 2.500000000000000000, 2.357898499370431722, -2.818925648462311528E-15 ) ) ;
#3511 = DIRECTION ( 'NONE',  ( 0.000000000000000000, 0.8090169943749487835, -0.5877852522924713607 ) ) ;
#3512 = EDGE_LOOP ( 'NONE', ( #12651, #7480, #13628, #17404 ) ) ;
#3513 = ADVANCED_FACE ( 'NONE', ( #9908 ), #15727, .F. ) ;
#3514 = DIRECTION ( 'NONE',  ( 0.9873298794253690946, -1.799126239882931805E-16, -0.1586811557617541224 ) ) ;
#3515 = AXIS2_PLACEMENT_3D ( 'NONE', #5370, #12419, #2424 ) ;
#3516 = EDGE_CURVE ( 'NONE', #7464, #15934, #5050, .T. ) ;
#3517 = VERTEX_POINT ( 'NONE', #15824 ) ;
#3518 = CARTESIAN_POINT ( 'NONE',  ( 0.000000000000000000, 0.000000000000000000, -4.694516984716113228 ) ) ;
#3519 = FACE_OUTER_BOUND ( 'NONE', #14329, .T. ) ;
#3520 = CIRCLE ( 'NONE', #14157, 0.2000000000000000944 ) ;
#3521 = VECTOR ( 'NONE', #1722, 1000.000000000000000 ) ;
#3522 = ADVANCED_FACE ( 'NONE', ( #3145 ), #7331, .T. ) ;
#3523 = AXIS2_PLACEMENT_3D ( 'NONE', #17027, #10809, #5291 ) ;
#3524 = VECTOR ( 'NONE', #16046, 1000.000000000000000 ) ;
#3525 = VERTEX_POINT ( 'NONE', #1345 ) ;
#3526 = EDGE_CURVE ( 'NONE', #2833, #9630, #18454, .T. ) ;
#3527 = AXIS2_PLACEMENT_3D ( 'NONE', #10794, #17012, #9660 ) ;
#3528 = ORIENTED_EDGE ( 'NONE', *, *, #18676, .F. ) ;
#3529 = DIRECTION ( 'NONE',  ( -1.000000000000000000, 0.000000000000000000, 0.000000000000000000 ) ) ;
#3530 = AXIS2_PLACEMENT_3D ( 'NONE', #15724, #12775, #17155 ) ;
#3531 = CARTESIAN_POINT ( 'NONE',  ( 0.000000000000000000, -24.79895094899250196, -13.40641754777691830 ) ) ;
#3532 = CARTESIAN_POINT ( 'NONE',  ( -12.50000000000000355, 0.000000000000000000, 0.000000000000000000 ) ) ;
#3533 = DIRECTION ( 'NONE',  ( -0.7071067811865254793, 0.000000000000000000, 0.7071067811865695552 ) ) ;
#3534 = CARTESIAN_POINT ( 'NONE',  ( 8.060728450267873768, -24.77235419320996357, -2.000000000000000000 ) ) ;
#3535 = ORIENTED_EDGE ( 'NONE', *, *, #18177, .F. ) ;
#3536 = CARTESIAN_POINT ( 'NONE',  ( 4.999999999999999112, -62.87238730325623948, 4.007856633823172032 ) ) ;
#3537 = EDGE_CURVE ( 'NONE', #6583, #16274, #15410, .T. ) ;
#3538 = ADVANCED_FACE ( 'NONE', ( #2774 ), #14750, .F. ) ;
#3539 =( NAMED_UNIT ( * ) PLANE_ANGLE_UNIT ( ) SI_UNIT ( $, .RADIAN. ) );
#3540 = DIRECTION ( 'NONE',  ( -1.000000000000000000, 0.000000000000000000, -0.000000000000000000 ) ) ;
#3541 = EDGE_LOOP ( 'NONE', ( #13369, #12246, #7203, #16130 ) ) ;
#3542 = AXIS2_PLACEMENT_3D ( 'NONE', #3849, #12226, #10888 ) ;
#3543 = AXIS2_PLACEMENT_3D ( 'NONE', #1433, #7237, #18 ) ;
#3544 = CONTEXT_DEPENDENT_SHAPE_REPRESENTATION ( #1258, #2080 ) ;
#3545 = EDGE_CURVE ( 'NONE', #4094, #15091, #5815, .T. ) ;
#3546 = ORIENTED_EDGE ( 'NONE', *, *, #10293, .T. ) ;
#3547 = AXIS2_PLACEMENT_3D ( 'NONE', #2118, #693, #12297 ) ;
#3548 = CIRCLE ( 'NONE', #16620, 63.00000000006298961 ) ;
#3549 = ADVANCED_FACE ( 'NONE', ( #18767 ), #1528, .F. ) ;
#3550 = ORIENTED_EDGE ( 'NONE', *, *, #427, .T. ) ;
#3551 = EDGE_LOOP ( 'NONE', ( #12645, #15066 ) ) ;
#3552 = ADVANCED_FACE ( 'NONE', ( #10010 ), #5902, .T. ) ;
#3553 = DIRECTION ( 'NONE',  ( 0.1305261922200524616, 0.9914448613738103822, -0.000000000000000000 ) ) ;
#3554 = DIRECTION ( 'NONE',  ( 0.000000000000000000, -0.3090169943749547787, 0.9510565162951511997 ) ) ;
#3555 = CIRCLE ( 'NONE', #1438, 56.24900000005626310 ) ;
#3556 = COLOUR_RGB ( '',1.000000000000000000, 0.9490196078431372140, 0.9098039215686274384 ) ;
#3557 = DIRECTION ( 'NONE',  ( 0.000000000000000000, 0.5877852522924685852, 0.8090169943749507819 ) ) ;
#3558 = CARTESIAN_POINT ( 'NONE',  ( -10.00000000000000000, 0.000000000000000000, 0.000000000000000000 ) ) ;
#3560 =( LENGTH_UNIT ( ) NAMED_UNIT ( * ) SI_UNIT ( .MILLI., .METRE. ) );
#3559 = AXIS2_PLACEMENT_3D ( 'NONE', #6389, #10947, #13724 ) ;
#3561 = DIRECTION ( 'NONE',  ( 0.000000000000000000, 0.000000000000000000, 1.000000000000000000 ) ) ;
#3562 = LINE ( 'NONE', #6217, #4642 ) ;
#3563 = CIRCLE ( 'NONE', #7209, 24.00000000002400569 ) ;
#3564 = MANIFOLD_SOLID_BREP ( 'Body', #4350 ) ;
#3565 = CARTESIAN_POINT ( 'NONE',  ( -79.64793068852898728, -38.00000000000000000, -29.21039329588757383 ) ) ;
#3566 = ORIENTED_EDGE ( 'NONE', *, *, #16168, .F. ) ;
#3567 = FACE_OUTER_BOUND ( 'NONE', #4961, .T. ) ;
#3568 = ORIENTED_EDGE ( 'NONE', *, *, #8794, .T. ) ;
#3569 = CARTESIAN_POINT ( 'NONE',  ( -10.00000000000000000, 0.000000000000000000, 0.000000000000000000 ) ) ;
#3570 = DIRECTION ( 'NONE',  ( 1.000000000000000000, 0.000000000000000000, 0.000000000000000000 ) ) ;
#3571 = CYLINDRICAL_SURFACE ( 'NONE', #5725, 27.50000000000000000 ) ;
#3572 = EDGE_LOOP ( 'NONE', ( #7108, #17752, #14808, #13191 ) ) ;
#3573 = ORIENTED_EDGE ( 'NONE', *, *, #3753, .T. ) ;
#3574 = CYLINDRICAL_SURFACE ( 'NONE', #4756, 63.00000000006298961 ) ;
#3575 = DIRECTION ( 'NONE',  ( 1.000000000000000000, 0.000000000000000000, 0.000000000000000000 ) ) ;
#3576 = FACE_OUTER_BOUND ( 'NONE', #7469, .T. ) ;
#3577 = ORIENTED_EDGE ( 'NONE', *, *, #10569, .T. ) ;
#3578 = CIRCLE ( 'NONE', #7219, 30.39999999999999858 ) ;
#3579 = EDGE_CURVE ( 'NONE', #13137, #2157, #12661, .T. ) ;
#3580 = AXIS2_PLACEMENT_3D ( 'NONE', #10279, #16091, #8843 ) ;
#3581 = AXIS2_PLACEMENT_3D ( 'NONE', #10797, #9186, #14816 ) ;
#3582 = AXIS2_PLACEMENT_3D ( 'NONE', #8174, #9587, #15407 ) ;
#3583 = DIRECTION ( 'NONE',  ( -1.000000000000000000, -0.000000000000000000, -0.000000000000000000 ) ) ;
#3584 = FACE_OUTER_BOUND ( 'NONE', #16769, .T. ) ;
#3585 = DIRECTION ( 'NONE',  ( 0.000000000000000000, 0.000000000000000000, -1.000000000000000000 ) ) ;
#3586 = ORIENTED_EDGE ( 'NONE', *, *, #13463, .F. ) ;
#3587 = CARTESIAN_POINT ( 'NONE',  ( 3.678949249685231848, 0.000000000000000000, 0.000000000000000000 ) ) ;
#3588 = CIRCLE ( 'NONE', #14236, 26.24900000002624978 ) ;
#3589 = VERTEX_POINT ( 'NONE', #2864 ) ;
#3590 = DIRECTION ( 'NONE',  ( 0.000000000000000000, 0.000000000000000000, 1.000000000000000000 ) ) ;
#3591 = ORIENTED_EDGE ( 'NONE', *, *, #5862, .F. ) ;
#3592 = FACE_OUTER_BOUND ( 'NONE', #5057, .T. ) ;
#3593 = DIRECTION ( 'NONE',  ( 0.000000000000000000, 0.000000000000000000, -1.000000000000000000 ) ) ;
#3594 = CIRCLE ( 'NONE', #2995, 56.24900000005625600 ) ;
#3595 = ORIENTED_EDGE ( 'NONE', *, *, #17059, .F. ) ;
#3596 = EDGE_LOOP ( 'NONE', ( #3401, #14385, #5873, #4656 ) ) ;
#3597 = CIRCLE ( 'NONE', #18186, 26.24900000002624978 ) ;
#3598 = FACE_OUTER_BOUND ( 'NONE', #5239, .T. ) ;
#3599 = ORIENTED_EDGE ( 'NONE', *, *, #12856, .T. ) ;
#3600 = DIRECTION ( 'NONE',  ( 0.000000000000000000, -0.4999999999999991118, 0.8660254037844390407 ) ) ;
#3601 = EDGE_CURVE ( 'NONE', #16476, #6965, #11748, .T. ) ;
#3602 = AXIS2_PLACEMENT_3D ( 'NONE', #2235, #5096, #6523 ) ;
#3603 = AXIS2_PLACEMENT_3D ( 'NONE', #17645, #14684, #399 ) ;
#3604 = CARTESIAN_POINT ( 'NONE',  ( 5.200000000000002842, 0.000000000000000000, 0.000000000000000000 ) ) ;
#3605 =( GEOMETRIC_REPRESENTATION_CONTEXT ( 3 ) GLOBAL_UNCERTAINTY_ASSIGNED_CONTEXT ( ( #8043 ) ) GLOBAL_UNIT_ASSIGNED_CONTEXT ( ( #1180, #17363, #14585 ) ) REPRESENTATION_CONTEXT ( 'NONE', 'WORKASPACE' ) );
#3606 = CIRCLE ( 'NONE', #16988, 56.24900000005627732 ) ;
#3607 = ORIENTED_EDGE ( 'NONE', *, *, #12237, .T. ) ;
#3608 = EDGE_LOOP ( 'NONE', ( #1027, #5900, #1607 ) ) ;
#3609 = CARTESIAN_POINT ( 'NONE',  ( 0.5449313310647804220, 4.304185902836899835, -3.316620875263383894 ) ) ;
#3610 = CARTESIAN_POINT ( 'NONE',  ( 10.00000000000000000, -4.007856633822949988, -62.87238730325625369 ) ) ;
#3611 = CARTESIAN_POINT ( 'NONE',  ( -79.64793068852898728, -30.00000000000000000, -29.21039329588758093 ) ) ;
#3612 = EDGE_CURVE ( 'NONE', #3711, #12567, #503, .T. ) ;
#3613 = VERTEX_POINT ( 'NONE', #16660 ) ;
#3614 = CYLINDRICAL_SURFACE ( 'NONE', #14823, 4.799999999999998934 ) ;
#3615 = DIRECTION ( 'NONE',  ( 0.000000000000000000, 1.000000000000000000, 0.000000000000000000 ) ) ;
#3616 = LINE ( 'NONE', #10827, #9810 ) ;
#3617 = AXIS2_PLACEMENT_3D ( 'NONE', #10139, #9261, #9170 ) ;
#3618 = CARTESIAN_POINT ( 'NONE',  ( 10.00000000000000178, 4.769696007084728073, 1.500000000000000000 ) ) ;
#3619 = ORIENTED_EDGE ( 'NONE', *, *, #6778, .F. ) ;
#3620 = CARTESIAN_POINT ( 'NONE',  ( 0.000000000000000000, -56.23315539212689629, -1.335003989222221410 ) ) ;
#3621 = AXIS2_PLACEMENT_3D ( 'NONE', #3147, #13344, #292 ) ;
#3622 = ADVANCED_FACE ( 'NONE', ( #9417 ), #464, .T. ) ;
#3623 =( BOUNDED_SURFACE ( )  B_SPLINE_SURFACE ( 3, 2, ( 
 ( #2384, #13143, #187 ),
 ( #5717, #17427, #1425 ),
 ( #1697, #3136, #281 ),
 ( #4378, #4560, #10181 ),
 ( #11805, #13332, #2767 ),
 ( #2857, #11532, #14744 ) ),
 .UNSPECIFIED., .F., .F., .F. ) 
 B_SPLINE_SURFACE_WITH_KNOTS ( ( 4, 2, 4 ),
 ( 3, 3 ),
 ( 0.02027752710269158445, 0.02273781595091097299, 0.02519810479913036153 ),
 ( 0.000000000000000000, 1.000000000000000000 ),
 .UNSPECIFIED. ) 
 GEOMETRIC_REPRESENTATION_ITEM ( )  RATIONAL_B_SPLINE_SURFACE ( (
 ( 1.000000000000000000, 0.8047781431712808242, 1.000000000000000000),
 ( 1.000000000000000000, 0.8123773247083928561, 1.000000000000000000),
 ( 1.000000000000000000, 0.8190670192154906326, 1.000000000000000000),
 ( 1.000000000000000000, 0.8192353552912178261, 1.000000000000000000),
 ( 1.000000000000000000, 0.8126132098226825917, 1.000000000000000000),
 ( 1.000000000000000000, 0.8047712465856394770, 1.000000000000000000) ) ) 
 REPRESENTATION_ITEM ( '' )  SURFACE ( )  );
#3624 = ORIENTED_EDGE ( 'NONE', *, *, #2685, .T. ) ;
#3625 = CARTESIAN_POINT ( 'NONE',  ( 10.00000000000000000, 24.46385708179996854, -9.514709542736643044 ) ) ;
#3626 = CARTESIAN_POINT ( 'NONE',  ( 10.00000000000000000, 5.940243314904674499, -32.46095361140685753 ) ) ;
#3627 = CIRCLE ( 'NONE', #14873, 56.24900000005625600 ) ;
#3628 = AXIS2_PLACEMENT_3D ( 'NONE', #15558, #8592, #9839 ) ;
#3629 = ORIENTED_EDGE ( 'NONE', *, *, #8452, .T. ) ;
#3630 = VECTOR ( 'NONE', #17416, 1000.000000000000000 ) ;
#3631 = ORIENTED_EDGE ( 'NONE', *, *, #12034, .F. ) ;
#3632 = CARTESIAN_POINT ( 'NONE',  ( 0.000000000000000000, 0.000000000000000000, 0.000000000000000000 ) ) ;
#3633 = FACE_BOUND ( 'NONE', #4197, .T. ) ;
#3634 = CARTESIAN_POINT ( 'NONE',  ( 10.00000000000000000, -27.72801475327278453, -5.086963483077506787 ) ) ;
#3635 = CARTESIAN_POINT ( 'NONE',  ( -26.29305231718584324, -26.50000000000000000, 19.10302069950530779 ) ) ;
#3636 = FACE_OUTER_BOUND ( 'NONE', #17621, .T. ) ;
#3637 = LINE ( 'NONE', #16777, #15094 ) ;
#3638 = ORIENTED_EDGE ( 'NONE', *, *, #7805, .F. ) ;
#3639 = CARTESIAN_POINT ( 'NONE',  ( -4.140404888673278272, -2.228338276487456415, -3.686887068327035166 ) ) ;
#3640 = SHAPE_REPRESENTATION_RELATIONSHIP ( 'NONE' , 'NONE' ,  #1770, #12609 ) ;
#3641 = PLANE ( 'NONE',  #12098 ) ;
#3642 = CIRCLE ( 'NONE', #3347, 25.00000000000000000 ) ;
#3643 = ORIENTED_EDGE ( 'NONE', *, *, #7218, .F. ) ;
#3644 = ORIENTED_EDGE ( 'NONE', *, *, #3420, .T. ) ;
#3645 = VERTEX_POINT ( 'NONE', #17795 ) ;
#3646 = EDGE_CURVE ( 'NONE', #11016, #6635, #4447, .T. ) ;
#3647 = ADVANCED_FACE ( 'NONE', ( #13713 ), #568, .T. ) ;
#3648 = ORIENTED_EDGE ( 'NONE', *, *, #1205, .F. ) ;
#3649 = CARTESIAN_POINT ( 'NONE',  ( -90.00000000009001155, -34.99999999999999289, -5.000000000000005329 ) ) ;
#3650 = ADVANCED_FACE ( 'NONE', ( #18078 ), #1983, .T. ) ;
#3651 = AXIS2_PLACEMENT_3D ( 'NONE', #8344, #10657, #16472 ) ;
#3652 = DIRECTION ( 'NONE',  ( 0.000000000000000000, 0.000000000000000000, 1.000000000000000000 ) ) ;
#3653 = DIRECTION ( 'NONE',  ( -0.000000000000000000, 1.000000000000000000, -0.000000000000000000 ) ) ;
#3654 = VECTOR ( 'NONE', #18615, 1000.000000000000000 ) ;
#3655 = EDGE_CURVE ( 'NONE', #12204, #4722, #1704, .T. ) ;
#3656 = FACE_OUTER_BOUND ( 'NONE', #1689, .T. ) ;
#3657 = DIRECTION ( 'NONE',  ( -1.000000000000000000, -0.000000000000000000, -0.000000000000000000 ) ) ;
#3658 = DIRECTION ( 'NONE',  ( 0.1305261922200524338, 0.9914448613738102711, 0.000000000000000000 ) ) ;
#3659 = VERTEX_POINT ( 'NONE', #6466 ) ;
#3660 = DIRECTION ( 'NONE',  ( 0.000000000000000000, 1.000000000000000000, 0.000000000000000000 ) ) ;
#3661 = ORIENTED_EDGE ( 'NONE', *, *, #16329, .F. ) ;
#3662 = CARTESIAN_POINT ( 'NONE',  ( 0.000000000000000000, 10.11537145609375443, 55.33199130079787409 ) ) ;
#3663 = FACE_OUTER_BOUND ( 'NONE', #2790, .T. ) ;
#3664 = VERTEX_POINT ( 'NONE', #15040 ) ;
#3665 = VERTEX_POINT ( 'NONE', #9035 ) ;
#3666 = CARTESIAN_POINT ( 'NONE',  ( -2.000000000000007550, -3.464101615137749945, 0.000000000000000000 ) ) ;
#3667 = DIRECTION ( 'NONE',  ( -4.953800363085478943E-17, -1.000000000000000000, 3.599146639029955428E-17 ) ) ;
#3668 = CARTESIAN_POINT ( 'NONE',  ( 34.99999999999999289, 0.000000000000000000, 0.000000000000000000 ) ) ;
#3669 = VERTEX_POINT ( 'NONE', #3426 ) ;
#3670 = EDGE_CURVE ( 'NONE', #12797, #5515, #5021, .T. ) ;
#3671 = AXIS2_PLACEMENT_3D ( 'NONE', #1644, #3274, #7361 ) ;
#3672 = AXIS2_PLACEMENT_3D ( 'NONE', #4965, #3739, #10769 ) ;
#3673 = ADVANCED_FACE ( 'NONE', ( #4752 ), #4659, .T. ) ;
#3674 = DIRECTION ( 'NONE',  ( 0.000000000000000000, 0.000000000000000000, 1.000000000000000000 ) ) ;
#3675 = CARTESIAN_POINT ( 'NONE',  ( 10.00000000000000000, -3.730438010304518492, 27.94286728106391138 ) ) ;
#3676 = CARTESIAN_POINT ( 'NONE',  ( -90.00000000009001155, -38.00000000000000000, 27.50000000000000000 ) ) ;
#3677 = VERTEX_POINT ( 'NONE', #6089 ) ;
#3678 = DIRECTION ( 'NONE',  ( -1.000000000000000000, -0.000000000000000000, -0.000000000000000000 ) ) ;
#3679 = EDGE_LOOP ( 'NONE', ( #8260, #18538, #18212, #10633 ) ) ;
#3680 = UNCERTAINTY_MEASURE_WITH_UNIT (LENGTH_MEASURE( 1.000000000000000082E-05 ), #8870, 'distance_accuracy_value', 'NONE');
#3681 = DIRECTION ( 'NONE',  ( -1.000000000000000000, 0.000000000000000000, 0.000000000000000000 ) ) ;
#3682 = EDGE_LOOP ( 'NONE', ( #2187, #18709, #11670, #10783 ) ) ;
#3683 = EDGE_CURVE ( 'NONE', #12720, #8736, #12354, .T. ) ;
#3684 = AXIS2_PLACEMENT_3D ( 'NONE', #13441, #13876, #16838 ) ;
#3685 = CARTESIAN_POINT ( 'NONE',  ( 2.000000000000008882, 3.464101615137749945, 0.000000000000000000 ) ) ;
#3686 = LINE ( 'NONE', #8252, #16214 ) ;
#3687 = VERTEX_POINT ( 'NONE', #7793 ) ;
#3688 = VERTEX_POINT ( 'NONE', #3620 ) ;
#3689 = DIRECTION ( 'NONE',  ( 0.000000000000000000, -1.000000000000000000, -1.047444401652940007E-14 ) ) ;
#3690 =( LENGTH_UNIT ( ) NAMED_UNIT ( * ) SI_UNIT ( .MILLI., .METRE. ) );
#3691 = ORIENTED_EDGE ( 'NONE', *, *, #15271, .T. ) ;
#3692 = DIRECTION ( 'NONE',  ( -0.000000000000000000, 1.000000000000000000, -0.000000000000000000 ) ) ;
#3693 = MANIFOLD_SOLID_BREP ( 'EndChamfer', #11944 ) ;
#3694 = CIRCLE ( 'NONE', #14042, 12.00000000001200462 ) ;
#3695 = CARTESIAN_POINT ( 'NONE',  ( 2.250000000000000000, -27.60846790388774608, -2.000000000000000000 ) ) ;
#3696 = CARTESIAN_POINT ( 'NONE',  ( 0.000000000000000000, 33.71303790549351476, -53.22058882792159551 ) ) ;
#3697 = ORIENTED_EDGE ( 'NONE', *, *, #11094, .T. ) ;
#3698 = ORIENTED_EDGE ( 'NONE', *, *, #12632, .F. ) ;
#3699 = CARTESIAN_POINT ( 'NONE',  ( 32.50000000000000000, -26.50000000000000000, 3.680389326632394941E-13 ) ) ;
#3700 = DIRECTION ( 'NONE',  ( -1.000000000000000000, 0.000000000000000000, 0.000000000000000000 ) ) ;
#3701 = DIRECTION ( 'NONE',  ( 0.000000000000000000, 0.8910065241883688980, -0.4539904997395446951 ) ) ;
#3702 = ORIENTED_EDGE ( 'NONE', *, *, #2980, .F. ) ;
#3703 = DIRECTION ( 'NONE',  ( -1.000000000000000000, 0.000000000000000000, -0.000000000000000000 ) ) ;
#3704 = EDGE_CURVE ( 'NONE', #8362, #11459, #16475, .T. ) ;
#3705 = EDGE_LOOP ( 'NONE', ( #16152, #4220 ) ) ;
#3706 = CARTESIAN_POINT ( 'NONE',  ( 0.000000000000000000, 0.000000000000000000, 0.000000000000000000 ) ) ;
#3707 = CARTESIAN_POINT ( 'NONE',  ( -79.64793068852927149, -34.99999999999999289, 31.86039329588764701 ) ) ;
#3708 = VERTEX_POINT ( 'NONE', #4941 ) ;
#3709 = EDGE_LOOP ( 'NONE', ( #8045, #7943, #2126, #3181 ) ) ;
#3710 = DIRECTION ( 'NONE',  ( 0.000000000000000000, 0.3090169943749481729, -0.9510565162951533091 ) ) ;
#3711 = VERTEX_POINT ( 'NONE', #16556 ) ;
#3712 = CARTESIAN_POINT ( 'NONE',  ( 10.00000000000000000, 20.32630374611185786, 16.60877409751175904 ) ) ;
#3713 = AXIS2_PLACEMENT_3D ( 'NONE', #3668, #18039, #7745 ) ;
#3714 = CARTESIAN_POINT ( 'NONE',  ( -85.22968676783801811, 1.000000000000018208, -0.5330212624288648282 ) ) ;
#3715 = AXIS2_PLACEMENT_3D ( 'NONE', #2940, #17238, #4370 ) ;
#3716 = EDGE_CURVE ( 'NONE', #16631, #845, #2324, .T. ) ;
#3717 = ORIENTED_EDGE ( 'NONE', *, *, #8148, .F. ) ;
#3718 = ADVANCED_FACE ( 'NONE', ( #2268 ), #15608, .T. ) ;
#3719 = CIRCLE ( 'NONE', #6141, 2.649999999999995914 ) ;
#3720 = VERTEX_POINT ( 'NONE', #760 ) ;
#3721 = FACE_OUTER_BOUND ( 'NONE', #18727, .T. ) ;
#3722 = FACE_BOUND ( 'NONE', #14975, .T. ) ;
#3723 = PLANE ( 'NONE',  #820 ) ;
#3724 = CYLINDRICAL_SURFACE ( 'NONE', #13903, 24.00000000002399858 ) ;
#3725 = AXIS2_PLACEMENT_3D ( 'NONE', #13222, #17604, #11795 ) ;
#3726 = CARTESIAN_POINT ( 'NONE',  ( 0.000000000000000000, 42.79754323328179311, -16.55576474687299537 ) ) ;
#3727 = CARTESIAN_POINT ( 'NONE',  ( 0.000000000000000000, -34.13306034420217827, 44.70888270294149436 ) ) ;
#3728 = EDGE_LOOP ( 'NONE', ( #5591, #5202, #10031, #15195 ) ) ;
#3729 = LINE ( 'NONE', #3536, #13656 ) ;
#3730 = DIRECTION ( 'NONE',  ( -1.000000000000000000, 0.000000000000000000, 0.000000000000000000 ) ) ;
#3731 = ORIENTED_EDGE ( 'NONE', *, *, #644, .F. ) ;
#3732 = VERTEX_POINT ( 'NONE', #6556 ) ;
#3733 = VECTOR ( 'NONE', #660, 1000.000000000000000 ) ;
#3734 = ORIENTED_EDGE ( 'NONE', *, *, #16685, .F. ) ;
#3735 = VECTOR ( 'NONE', #12593, 1000.000000000000000 ) ;
#3736 = VECTOR ( 'NONE', #7421, 1000.000000000000000 ) ;
#3737 = ORIENTED_EDGE ( 'NONE', *, *, #17718, .F. ) ;
#3738 = DIRECTION ( 'NONE',  ( -1.000000000000000000, 0.000000000000000000, 0.000000000000000000 ) ) ;
#3739 = DIRECTION ( 'NONE',  ( -0.000000000000000000, 1.000000000000000000, 1.224646799147353207E-16 ) ) ;
#3740 = CARTESIAN_POINT ( 'NONE',  ( 10.04305231718579705, -34.99999999999999289, 28.25933677959249835 ) ) ;
#3741 = CARTESIAN_POINT ( 'NONE',  ( 5.000000000000000888, 0.000000000000000000, 0.000000000000000000 ) ) ;
#3742 = CARTESIAN_POINT ( 'NONE',  ( -1.250000000000000000, -6.429618962271402616, -1.000000000000000000 ) ) ;
#3743 = DIRECTION ( 'NONE',  ( 0.000000000000000000, 0.000000000000000000, 1.000000000000000000 ) ) ;
#3744 = DIRECTION ( 'NONE',  ( -1.000000000000000000, 0.000000000000000000, 0.000000000000000000 ) ) ;
#3745 = ORIENTED_EDGE ( 'NONE', *, *, #162, .T. ) ;
#3746 = LINE ( 'NONE', #18399, #9996 ) ;
#3747 = ORIENTED_EDGE ( 'NONE', *, *, #6030, .F. ) ;
#3748 = CARTESIAN_POINT ( 'NONE',  ( -90.00000000009001155, 2.081668171172168513E-14, -1.301042606982603940E-15 ) ) ;
#3749 = DIRECTION ( 'NONE',  ( -1.000000000000000000, -0.000000000000000000, -0.000000000000000000 ) ) ;
#3750 = ORIENTED_EDGE ( 'NONE', *, *, #9344, .T. ) ;
#3751 = EDGE_LOOP ( 'NONE', ( #10528, #15735, #13331, #7986 ) ) ;
#3752 = AXIS2_PLACEMENT_3D ( 'NONE', #13716, #11986, #16559 ) ;
#3753 = EDGE_CURVE ( 'NONE', #18350, #4490, #9626, .T. ) ;
#3754 = DIRECTION ( 'NONE',  ( 1.000000000000000000, 0.000000000000000000, 0.000000000000000000 ) ) ;
#3755 = DIRECTION ( 'NONE',  ( -0.8090169943749422332, 6.123233995736766036E-17, -0.5877852522924802425 ) ) ;
#3757 = EDGE_CURVE ( 'NONE', #12242, #8620, #3855, .T. ) ;
#3756 = DIRECTION ( 'NONE',  ( 0.000000000000000000, 0.000000000000000000, -1.000000000000000000 ) ) ;
#3758 = VERTEX_POINT ( 'NONE', #3995 ) ;
#3759 = PRODUCT_RELATED_PRODUCT_CATEGORY ( 'part', '', ( #8742 ) ) ;
#3760 = ADVANCED_FACE ( 'NONE', ( #18178 ), #12558, .T. ) ;
#3761 = CIRCLE ( 'NONE', #3149, 5.000000000000004441 ) ;
#3762 = LINE ( 'NONE', #817, #15706 ) ;
#3763 = PLANE ( 'NONE',  #9122 ) ;
#3764 = DIRECTION ( 'NONE',  ( 0.000000000000000000, 1.000000000000000000, 0.000000000000000000 ) ) ;
#3765 = ORIENTED_EDGE ( 'NONE', *, *, #7823, .T. ) ;
#3766 = CARTESIAN_POINT ( 'NONE',  ( 10.00000000000000000, 0.000000000000000000, 0.000000000000000000 ) ) ;
#3767 = EDGE_CURVE ( 'NONE', #6042, #8506, #214, .T. ) ;
#3768 = ORIENTED_EDGE ( 'NONE', *, *, #4807, .T. ) ;
#3769 = DIRECTION ( 'NONE',  ( 0.000000000000000000, 0.000000000000000000, -1.000000000000000000 ) ) ;
#3770 = ORIENTED_EDGE ( 'NONE', *, *, #2590, .T. ) ;
#3771 = CARTESIAN_POINT ( 'NONE',  ( -26.29305231718568336, -30.00000000000000000, -19.10302069950552095 ) ) ;
#3772 = DIRECTION ( 'NONE',  ( -1.000000000000000000, 0.000000000000000000, 0.000000000000000000 ) ) ;
#3773 = CARTESIAN_POINT ( 'NONE',  ( 5.200000000000002842, 0.000000000000000000, 0.000000000000000000 ) ) ;
#3774 = ORIENTED_EDGE ( 'NONE', *, *, #2555, .T. ) ;
#3775 = ORIENTED_EDGE ( 'NONE', *, *, #15862, .T. ) ;
#3776 = EDGE_CURVE ( 'NONE', #16740, #16445, #11228, .T. ) ;
#3777 = CARTESIAN_POINT ( 'NONE',  ( 10.00000000000000000, 46.20417134726132247, 32.31183295104789011 ) ) ;
#3778 = ADVANCED_FACE ( 'NONE', ( #2464 ), #8368, .T. ) ;
#3779 = EDGE_LOOP ( 'NONE', ( #4322, #17968, #9789, #10153 ) ) ;
#3780 = DIRECTION ( 'NONE',  ( 0.000000000000000000, 0.000000000000000000, 1.000000000000000000 ) ) ;
#3781 = ADVANCED_FACE ( 'NONE', ( #10935 ), #14176, .T. ) ;
#3782 = EDGE_CURVE ( 'NONE', #17821, #6186, #12372, .T. ) ;
#3783 = PLANE ( 'NONE',  #16288 ) ;
#3784 = CARTESIAN_POINT ( 'NONE',  ( 0.000000000000000000, 32.31183295104839459, -46.20417134726096009 ) ) ;
#3785 = EDGE_LOOP ( 'NONE', ( #10703, #14581, #9081, #11061 ) ) ;
#3786 = DIRECTION ( 'NONE',  ( -0.000000000000000000, 1.000000000000000000, -0.000000000000000000 ) ) ;
#3787 = ORIENTED_EDGE ( 'NONE', *, *, #5143, .F. ) ;
#3788 = CARTESIAN_POINT ( 'NONE',  ( 5.000000000000002665, 0.000000000000000000, -2.700000000000000622 ) ) ;
#3789 = CARTESIAN_POINT ( 'NONE',  ( 0.000000000000000000, -16.60877409751182654, 20.32630374611179391 ) ) ;
#3790 = DIRECTION ( 'NONE',  ( 0.000000000000000000, 1.000000000000000000, 3.491481338843133355E-15 ) ) ;
#3791 = ORIENTED_EDGE ( 'NONE', *, *, #1967, .F. ) ;
#3792 = CARTESIAN_POINT ( 'NONE',  ( 10.00000000000000000, 50.71018745830478736, -24.33982105418846942 ) ) ;
#3793 = ORIENTED_EDGE ( 'NONE', *, *, #8448, .T. ) ;
#3794 = DIRECTION ( 'NONE',  ( -1.000000000000000000, -0.000000000000000000, 0.000000000000000000 ) ) ;
#3795 = DIRECTION ( 'NONE',  ( 0.000000000000000000, 0.000000000000000000, 1.000000000000000000 ) ) ;
#3796 = ORIENTED_EDGE ( 'NONE', *, *, #12383, .F. ) ;
#3797 = ORIENTED_EDGE ( 'NONE', *, *, #7458, .F. ) ;
#3798 = ORIENTED_EDGE ( 'NONE', *, *, #2685, .F. ) ;
#3799 = LINE ( 'NONE', #3712, #12737 ) ;
#3800 = CARTESIAN_POINT ( 'NONE',  ( -2.100000000000000089, 2.571758278209441957E-16, -5.000000000000000000 ) ) ;
#3801 = STYLED_ITEM ( 'NONE', ( #16053 ), #13523 ) ;
#3802 = AXIS2_PLACEMENT_3D ( 'NONE', #1057, #15626, #14300 ) ;
#3803 = AXIS2_PLACEMENT_3D ( 'NONE', #10925, #16749, #2170 ) ;
#3804 = EDGE_CURVE ( 'NONE', #16545, #11178, #1132, .T. ) ;
#3805 = MANIFOLD_SOLID_BREP ( 'Hex', #18036 ) ;
#3806 = ORIENTED_EDGE ( 'NONE', *, *, #11750, .F. ) ;
#3807 = EDGE_LOOP ( 'NONE', ( #8476, #5920, #10354, #6113 ) ) ;
#3808 = DIRECTION ( 'NONE',  ( 1.000000000000000000, -0.000000000000000000, 0.000000000000000000 ) ) ;
#3809 = CARTESIAN_POINT ( 'NONE',  ( 5.032868406504333869, -28.36021363089093938, -2.000000000000000000 ) ) ;
#3810 = FACE_OUTER_BOUND ( 'NONE', #14253, .T. ) ;
#3811 = DIRECTION ( 'NONE',  ( -1.000000000000000000, 0.000000000000000000, 0.000000000000000000 ) ) ;
#3812 = AXIS2_PLACEMENT_3D ( 'NONE', #17545, #393, #4772 ) ;
#3813 = CARTESIAN_POINT ( 'NONE',  ( 4.000000000000000000, 2.309401076758497151, -5.000000000000000000 ) ) ;
#3814 = DIRECTION ( 'NONE',  ( -1.000000000000000000, 0.000000000000000000, 0.000000000000000000 ) ) ;
#3815 = AXIS2_PLACEMENT_3D ( 'NONE', #7500, #17693, #4643 ) ;
#3816 = CYLINDRICAL_SURFACE ( 'NONE', #7792, 24.00000000002399858 ) ;
#3817 = VERTEX_POINT ( 'NONE', #3901 ) ;
#3818 = LINE ( 'NONE', #11045, #5135 ) ;
#3819 = AXIS2_PLACEMENT_3D ( 'NONE', #1746, #14357, #9168 ) ;
#3820 = FACE_OUTER_BOUND ( 'NONE', #9248, .T. ) ;
#3821 = DIRECTION ( 'NONE',  ( 0.000000000000000000, 0.000000000000000000, 1.000000000000000000 ) ) ;
#3822 = ORIENTED_EDGE ( 'NONE', *, *, #2944, .T. ) ;
#3823 = AXIS2_PLACEMENT_3D ( 'NONE', #14060, #6530, #11095 ) ;
#3824 = EDGE_CURVE ( 'NONE', #14293, #5713, #15322, .T. ) ;
#3825 = ORIENTED_EDGE ( 'NONE', *, *, #9715, .F. ) ;
#3826 = AXIS2_PLACEMENT_3D ( 'NONE', #11298, #13872, #16743 ) ;
#3827 = AXIS2_PLACEMENT_3D ( 'NONE', #15746, #9746, #17368 ) ;
#3828 = VERTEX_POINT ( 'NONE', #5604 ) ;
#3829 = DIRECTION ( 'NONE',  ( -0.000000000000000000, -1.000000000000000000, -0.000000000000000000 ) ) ;
#3830 = DIRECTION ( 'NONE',  ( 0.000000000000000000, 0.000000000000000000, -1.000000000000000000 ) ) ;
#3831 = DIRECTION ( 'NONE',  ( 1.000000000000000000, 0.000000000000000000, 0.000000000000000000 ) ) ;
#3832 = CYLINDRICAL_SURFACE ( 'NONE', #5153, 24.00000000002399858 ) ;
#3833 = CARTESIAN_POINT ( 'NONE',  ( 0.000000000000000000, -32.31183295104739273, -46.20417134726167063 ) ) ;
#3834 = CARTESIAN_POINT ( 'NONE',  ( 10.00000000000000000, -53.29895248911688554, 18.38754094778222026 ) ) ;
#3835 = CIRCLE ( 'NONE', #5962, 25.00000000000000000 ) ;
#3836 = CARTESIAN_POINT ( 'NONE',  ( 10.00000000000000000, 49.76630880786309064, 26.49895292618021614 ) ) ;
#3837 = VERTEX_POINT ( 'NONE', #7113 ) ;
#3838 = CARTESIAN_POINT ( 'NONE',  ( 10.00000000000000000, 3.730438010304324425, 27.94286728106393980 ) ) ;
#3839=STYLED_ITEM('',(#18876),#3243);
#3840 = EDGE_LOOP ( 'NONE', ( #10422, #1041, #1900, #11359 ) ) ;
#3841 = EDGE_CURVE ( 'NONE', #980, #15243, #18152, .T. ) ;
#3842 = CIRCLE ( 'NONE', #16304, 24.00000000002400213 ) ;
#3843 = FACE_OUTER_BOUND ( 'NONE', #17898, .T. ) ;
#3844 = PLANE ( 'NONE',  #10575 ) ;
#3845 = ORIENTED_EDGE ( 'NONE', *, *, #16410, .T. ) ;
#3846 = VECTOR ( 'NONE', #18525, 1000.000000000000000 ) ;
#3847 = ORIENTED_EDGE ( 'NONE', *, *, #17063, .T. ) ;
#3848 = VECTOR ( 'NONE', #12673, 1000.000000000000000 ) ;
#3849 = CARTESIAN_POINT ( 'NONE',  ( 10.00000000000000000, 53.92768374110892893, -16.45250512421876010 ) ) ;
#3850 =( NAMED_UNIT ( * ) SI_UNIT ( $, .STERADIAN. ) SOLID_ANGLE_UNIT ( ) );
#3851 = ADVANCED_FACE ( 'NONE', ( #2928 ), #8735, .T. ) ;
#3852 = LINE ( 'NONE', #15198, #10033 ) ;
#3853 = ORIENTED_EDGE ( 'NONE', *, *, #1557, .F. ) ;
#3854 = AXIS2_PLACEMENT_3D ( 'NONE', #1518, #8566, #5530 ) ;
#3855 = CIRCLE ( 'NONE', #12946, 12.00000000001200640 ) ;
#3856 = AXIS2_PLACEMENT_3D ( 'NONE', #3532, #13809, #15332 ) ;
#3857 = CARTESIAN_POINT ( 'NONE',  ( 10.00000000000000000, 56.37237871411034007, 25.01730853553658207 ) ) ;
#3858 = CARTESIAN_POINT ( 'NONE',  ( 0.000000000000000000, 61.47135697633798657, -13.79392154159068262 ) ) ;
#3859 = AXIS2_PLACEMENT_3D ( 'NONE', #2297, #9446, #15344 ) ;
#3860 = AXIS2_PLACEMENT_3D ( 'NONE', #4098, #14092, #14296 ) ;
#3861 = DIRECTION ( 'NONE',  ( 0.000000000000000000, 0.000000000000000000, 1.000000000000000000 ) ) ;
#3862 = FACE_OUTER_BOUND ( 'NONE', #3011, .T. ) ;
#3863 = ADVANCED_FACE ( 'NONE', ( #12937 ), #5796, .T. ) ;
#3864 = ORIENTED_EDGE ( 'NONE', *, *, #17557, .F. ) ;
#3865 = DIRECTION ( 'NONE',  ( -1.000000000000000000, -0.000000000000000000, -0.000000000000000000 ) ) ;
#3866 = ORIENTED_EDGE ( 'NONE', *, *, #12739, .F. ) ;
#3867 = CARTESIAN_POINT ( 'NONE',  ( 10.00000000000000000, 0.000000000000000000, 0.000000000000000000 ) ) ;
#3868 = DIRECTION ( 'NONE',  ( -1.000000000000000000, 0.000000000000000000, 0.000000000000000000 ) ) ;
#3869 = CARTESIAN_POINT ( 'NONE',  ( 10.00000000000000000, 0.000000000000000000, 0.000000000000000000 ) ) ;
#3870 = AXIS2_PLACEMENT_3D ( 'NONE', #11885, #6458, #13612 ) ;
#3871 = ORIENTED_EDGE ( 'NONE', *, *, #14108, .F. ) ;
#3872 = ORIENTED_EDGE ( 'NONE', *, *, #6706, .T. ) ;
#3873 = DIRECTION ( 'NONE',  ( 0.000000000000000000, 0.9510565162951523099, 0.3090169943749516701 ) ) ;
#3874 = VECTOR ( 'NONE', #9306, 1000.000000000000000 ) ;
#3875 = VERTEX_POINT ( 'NONE', #1239 ) ;
#3876 = CARTESIAN_POINT ( 'NONE',  ( 0.4999999999999916733, -30.39588787977742257, 0.000000000000000000 ) ) ;
#3877 = VECTOR ( 'NONE', #10817, 1000.000000000000000 ) ;
#3878 = CARTESIAN_POINT ( 'NONE',  ( 0.000000000000000000, -25.42247726998005675, -12.18267823974779240 ) ) ;
#3879 = AXIS2_PLACEMENT_3D ( 'NONE', #16179, #3134, #6786 ) ;
#3880 = DIRECTION ( 'NONE',  ( -0.5000000000000019984, -0.8660254037844375974, 0.000000000000000000 ) ) ;
#3881 = EDGE_CURVE ( 'NONE', #445, #12447, #5882, .T. ) ;
#3882 = EDGE_LOOP ( 'NONE', ( #17815, #1589, #7518, #2048 ) ) ;
#3883 = EDGE_CURVE ( 'NONE', #16268, #4068, #5652, .T. ) ;
#3884 = LINE ( 'NONE', #13981, #4583 ) ;
#3885 = AXIS2_PLACEMENT_3D ( 'NONE', #17001, #3954, #5176 ) ;
#3886 = ADVANCED_FACE ( 'NONE', ( #1594 ), #784, .F. ) ;
#3887 = VECTOR ( 'NONE', #11680, 1000.000000000000000 ) ;
#3888 = VERTEX_POINT ( 'NONE', #11406 ) ;
#3889 = CARTESIAN_POINT ( 'NONE',  ( 1.274258131564866448, 3.883108878240963513, -3.220599429844046568 ) ) ;
#3890 = VECTOR ( 'NONE', #7156, 1000.000000000000000 ) ;
#3891 = CARTESIAN_POINT ( 'NONE',  ( -4.144923636027600722, -29.35885059145708098, -2.000000000000000000 ) ) ;
#3892 = CARTESIAN_POINT ( 'NONE',  ( 10.00000000000000000, 31.97297851452424311, 46.27827401617415148 ) ) ;
#3893 = VERTEX_POINT ( 'NONE', #17229 ) ;
#3894 = CARTESIAN_POINT ( 'NONE',  ( -4.000000000000000000, -2.309401076758515803, -0.4999999999999995559 ) ) ;
#3895 = VERTEX_POINT ( 'NONE', #14548 ) ;
#3896 = EDGE_CURVE ( 'NONE', #18659, #13886, #16585, .T. ) ;
#3897 = CARTESIAN_POINT ( 'NONE',  ( 4.999999999999997335, 0.000000000000000000, 4.250000000000000000 ) ) ;
#3898 = CARTESIAN_POINT ( 'NONE',  ( 10.00000000000000000, 27.72801475327274900, 5.086963483077687975 ) ) ;
#3899 = ORIENTED_EDGE ( 'NONE', *, *, #15357, .F. ) ;
#3900 = ORIENTED_EDGE ( 'NONE', *, *, #18325, .T. ) ;
#3901 = CARTESIAN_POINT ( 'NONE',  ( -12.50000000000000355, 3.306546357697854128E-15, 27.00000000000000355 ) ) ;
#3902 = EDGE_CURVE ( 'NONE', #13064, #9389, #5018, .T. ) ;
#3903 = ORIENTED_EDGE ( 'NONE', *, *, #7498, .F. ) ;
#3904 = CARTESIAN_POINT ( 'NONE',  ( 10.00000000000000000, 12.18267823974788122, -25.42247726998001411 ) ) ;
#3905 = ADVANCED_FACE ( 'NONE', ( #17332 ), #13129, .F. ) ;
#3906 = CARTESIAN_POINT ( 'NONE',  ( 10.00000000000000000, 0.000000000000000000, 0.000000000000000000 ) ) ;
#3907 = CIRCLE ( 'NONE', #6626, 4.799999999999998934 ) ;
#3908 = VECTOR ( 'NONE', #3730, 1000.000000000000000 ) ;
#3909 = ADVANCED_FACE ( 'NONE', ( #17498 ), #8555, .T. ) ;
#3910 = AXIS2_PLACEMENT_3D ( 'NONE', #9951, #17193, #5663 ) ;
#3911 = VECTOR ( 'NONE', #5236, 1000.000000000000000 ) ;
#3912 = ORIENTED_EDGE ( 'NONE', *, *, #4023, .T. ) ;
#3913 = EDGE_CURVE ( 'NONE', #12565, #11990, #10262, .T. ) ;
#3914 = CIRCLE ( 'NONE', #7546, 24.00000000002399858 ) ;
#3915 = ORIENTED_EDGE ( 'NONE', *, *, #5033, .T. ) ;
#3916 = FACE_BOUND ( 'NONE', #16355, .T. ) ;
#3917 = CARTESIAN_POINT ( 'NONE',  ( 4.000000000001088907, 1.658577278524410170, -3.531553309554541720 ) ) ;
#3918 = CARTESIAN_POINT ( 'NONE',  ( 10.00000000000000000, 45.00825343885067298, -33.95787273855199828 ) ) ;
#3919 = DIRECTION ( 'NONE',  ( -1.000000000000000000, -0.000000000000000000, -0.000000000000000000 ) ) ;
#3920 = CIRCLE ( 'NONE', #7247, 4.000000000000000000 ) ;
#3921 = DIRECTION ( 'NONE',  ( 1.000000000000000000, 0.000000000000000000, 0.000000000000000000 ) ) ;
#3922 = CARTESIAN_POINT ( 'NONE',  ( 0.000000000000000000, 0.000000000000000000, -2.000000000000000000 ) ) ;
#3923 = AXIS2_PLACEMENT_3D ( 'NONE', #900, #5064, #1073 ) ;
#3924 = DIRECTION ( 'NONE',  ( 0.000000000000000000, 0.000000000000000000, -1.000000000000000000 ) ) ;
#3925 = ORIENTED_EDGE ( 'NONE', *, *, #3441, .F. ) ;
#3926 = VECTOR ( 'NONE', #18361, 1000.000000000000000 ) ;
#3927 = FACE_OUTER_BOUND ( 'NONE', #1791, .T. ) ;
#3928 = ADVANCED_FACE ( 'NONE', ( #1408 ), #2839, .T. ) ;
#3929 = DIRECTION ( 'NONE',  ( -1.000000000000000000, -0.000000000000000000, -0.000000000000000000 ) ) ;
#3930 = DIRECTION ( 'NONE',  ( -1.000000000000000000, 0.000000000000000000, -0.000000000000000000 ) ) ;
#3931 = DIRECTION ( 'NONE',  ( -0.000000000000000000, -1.000000000000000000, -0.000000000000000000 ) ) ;
#3932 = CONTEXT_DEPENDENT_SHAPE_REPRESENTATION ( #15593, #555 ) ;
#3933 = ORIENTED_EDGE ( 'NONE', *, *, #7356, .T. ) ;
#3934 = VECTOR ( 'NONE', #10500, 1000.000000000000000 ) ;
#3935 = CIRCLE ( 'NONE', #13976, 2.649999999999999467 ) ;
#3936 = ORIENTED_EDGE ( 'NONE', *, *, #18440, .F. ) ;
#3937 = AXIS2_PLACEMENT_3D ( 'NONE', #15097, #812, #13574 ) ;
#3938 = AXIS2_PLACEMENT_3D ( 'NONE', #5140, #876, #15434 ) ;
#3939 = ORIENTED_EDGE ( 'NONE', *, *, #7905, .F. ) ;
#3940 = DIRECTION ( 'NONE',  ( 0.000000000000000000, 1.000000000000000000, 0.000000000000000000 ) ) ;
#3941 = FILL_AREA_STYLE ('',( #2407 ) ) ;
#3942 = CARTESIAN_POINT ( 'NONE',  ( -11.15000000000000391, 0.000000000000000000, 0.000000000000000000 ) ) ;
#3943 = DIRECTION ( 'NONE',  ( 0.000000000000000000, 0.000000000000000000, 1.000000000000000000 ) ) ;
#3944 = CARTESIAN_POINT ( 'NONE',  ( 32.50000000000000000, -26.50000000000000000, -2.649999999999631317 ) ) ;
#3945 = VECTOR ( 'NONE', #14406, 1000.000000000000000 ) ;
#3946 = CARTESIAN_POINT ( 'NONE',  ( 0.000000000000000000, -30.00000000000000000, 0.000000000000000000 ) ) ;
#3947 = DIRECTION ( 'NONE',  ( 0.000000000000000000, 0.000000000000000000, 1.000000000000000000 ) ) ;
#3948 = ORIENTED_EDGE ( 'NONE', *, *, #16216, .T. ) ;
#3949 = LINE ( 'NONE', #15084, #17906 ) ;
#3950 = ORIENTED_EDGE ( 'NONE', *, *, #14984, .F. ) ;
#3951 = EDGE_CURVE ( 'NONE', #9406, #3665, #16632, .T. ) ;
#3952 = AXIS2_PLACEMENT_3D ( 'NONE', #6731, #1215, #4069 ) ;
#3953 = DIRECTION ( 'NONE',  ( -1.000000000000000000, 0.000000000000000000, 0.000000000000000000 ) ) ;
#3954 = DIRECTION ( 'NONE',  ( -0.000000000000000000, 0.000000000000000000, 1.000000000000000000 ) ) ;
#3955 = ORIENTED_EDGE ( 'NONE', *, *, #5499, .T. ) ;
#3956 = VERTEX_POINT ( 'NONE', #7399 ) ;
#3957 = DIRECTION ( 'NONE',  ( -1.000000000000000000, 0.000000000000000000, -0.000000000000000000 ) ) ;
#3958 = APPLICATION_PROTOCOL_DEFINITION ( 'draft international standard', 'automotive_design', 1998, #1708 ) ;
#3959 = CARTESIAN_POINT ( 'NONE',  ( 0.000000000000000000, -56.37237871411034718, 1.017308535512174261 ) ) ;
#3960 = VERTEX_POINT ( 'NONE', #13216 ) ;
#3961 = VECTOR ( 'NONE', #2481, 1000.000000000000000 ) ;
#3962 = DIRECTION ( 'NONE',  ( -1.000000000000000000, 0.000000000000000000, -0.000000000000000000 ) ) ;
#3963 = CARTESIAN_POINT ( 'NONE',  ( 34.99999999999999289, 0.000000000000000000, 2.055000000000000160 ) ) ;
#3964 = DIRECTION ( 'NONE',  ( 1.000000000000000000, 0.000000000000000000, 0.000000000000000000 ) ) ;
#3965 = DIRECTION ( 'NONE',  ( 0.000000000000000000, 0.000000000000000000, 1.000000000000000000 ) ) ;
#3966 = EDGE_CURVE ( 'NONE', #16722, #9159, #4728, .T. ) ;
#3967 = DIRECTION ( 'NONE',  ( 0.000000000000000000, 0.000000000000000000, 1.000000000000000000 ) ) ;
#3968 = ORIENTED_EDGE ( 'NONE', *, *, #2019, .F. ) ;
#3969 = CARTESIAN_POINT ( 'NONE',  ( -90.00000000009001155, -30.00000000000000000, 10.00000000000000711 ) ) ;
#3970 = CARTESIAN_POINT ( 'NONE',  ( 0.000000000000000000, 0.000000000000000000, 0.000000000000000000 ) ) ;
#3971 = CARTESIAN_POINT ( 'NONE',  ( 5.000000000000000000, 48.50907078259382388, 40.19788616105627455 ) ) ;
#3972 = ORIENTED_EDGE ( 'NONE', *, *, #9995, .T. ) ;
#3973 = ORIENTED_EDGE ( 'NONE', *, *, #16131, .T. ) ;
#3974 = VECTOR ( 'NONE', #14333, 1000.000000000000000 ) ;
#3975 = FACE_BOUND ( 'NONE', #256, .T. ) ;
#3976 = VECTOR ( 'NONE', #9661, 1000.000000000000114 ) ;
#3977 = ORIENTED_EDGE ( 'NONE', *, *, #42, .T. ) ;
#3978 = CARTESIAN_POINT ( 'NONE',  ( 10.00000000000000000, -1.489278925039337453, -26.20671763660629949 ) ) ;
#3979 = CARTESIAN_POINT ( 'NONE',  ( 10.00000000000000000, 0.000000000000000000, 0.000000000000000000 ) ) ;
#3980 = LINE ( 'NONE', #2538, #8124 ) ;
#3981 = ORIENTED_EDGE ( 'NONE', *, *, #10266, .F. ) ;
#3983 = VECTOR ( 'NONE', #12117, 1000.000000000000000 ) ;
#3982 = LINE ( 'NONE', #18447, #1852 ) ;
#3984 = ORIENTED_EDGE ( 'NONE', *, *, #6193, .F. ) ;
#3985 = DIRECTION ( 'NONE',  ( 0.000000000000000000, 0.000000000000000000, 1.000000000000000000 ) ) ;
#3986 = LINE ( 'NONE', #18554, #12561 ) ;
#3987 = CARTESIAN_POINT ( 'NONE',  ( -90.00000000009003998, 1.000000000000018208, -5.746271514173173500E-15 ) ) ;
#3988 = VERTEX_POINT ( 'NONE', #9887 ) ;
#3989 = DIRECTION ( 'NONE',  ( 0.000000000000000000, 0.000000000000000000, 1.000000000000000000 ) ) ;
#3990 = EDGE_LOOP ( 'NONE', ( #314, #6403, #15120, #15749 ) ) ;
#3991 = DIRECTION ( 'NONE',  ( 0.000000000000000000, 0.000000000000000000, 1.000000000000000000 ) ) ;
#3992 = CARTESIAN_POINT ( 'NONE',  ( 0.000000000000000000, 3.730438010304324425, 27.94286728106393980 ) ) ;
#3993 = VERTEX_POINT ( 'NONE', #6250 ) ;
#3994 = VERTEX_POINT ( 'NONE', #1963 ) ;
#3995 = CARTESIAN_POINT ( 'NONE',  ( 10.00000000000000000, 23.88582760061514421, -22.76987570971500929 ) ) ;
#3996 =( NAMED_UNIT ( * ) PLANE_ANGLE_UNIT ( ) SI_UNIT ( $, .RADIAN. ) );
#3997 = ORIENTED_EDGE ( 'NONE', *, *, #10814, .F. ) ;
#3998 = DIRECTION ( 'NONE',  ( 0.000000000000000000, 0.000000000000000000, 1.000000000000000000 ) ) ;
#3999 = CARTESIAN_POINT ( 'NONE',  ( 10.00000000000000000, -62.87238730325617553, -4.007856633824042447 ) ) ;
#4000 = EDGE_CURVE ( 'NONE', #3993, #16544, #9199, .T. ) ;
#4001 = AXIS2_PLACEMENT_3D ( 'NONE', #12977, #11636, #8675 ) ;
#4002 = EDGE_CURVE ( 'NONE', #12565, #195, #14810, .T. ) ;
#4003 = EDGE_CURVE ( 'NONE', #5560, #7581, #18722, .T. ) ;
#4004 = ORIENTED_EDGE ( 'NONE', *, *, #14408, .F. ) ;
#4005 = EDGE_CURVE ( 'NONE', #5290, #9292, #17877, .T. ) ;
#4006 = ORIENTED_EDGE ( 'NONE', *, *, #16784, .F. ) ;
#4007 = CYLINDRICAL_SURFACE ( 'NONE', #6593, 24.00000000002399858 ) ;
#4008 = DIRECTION ( 'NONE',  ( 0.000000000000000000, 0.000000000000000000, 1.000000000000000000 ) ) ;
#4009 = DIRECTION ( 'NONE',  ( 0.000000000000000000, 0.000000000000000000, 1.000000000000000000 ) ) ;
#4010 = CARTESIAN_POINT ( 'NONE',  ( 5.000000000000000000, 15.61693798565582547, -61.03368945066419826 ) ) ;
#4011 = VECTOR ( 'NONE', #5766, 1000.000000000000114 ) ;
#4012 = ADVANCED_FACE ( 'NONE', ( #13596 ), #4833, .T. ) ;
#4013 = DIRECTION ( 'NONE',  ( 0.000000000000000000, -0.8910065241883626808, -0.4539904997395568520 ) ) ;
#4014 = DIRECTION ( 'NONE',  ( -1.000000000000000000, -0.000000000000000000, -0.000000000000000000 ) ) ;
#4015 = CARTESIAN_POINT ( 'NONE',  ( 5.000000000000000000, 58.55669782892461939, 23.24033432160458545 ) ) ;
#4016 = ORIENTED_EDGE ( 'NONE', *, *, #10056, .T. ) ;
#4017 = FACE_OUTER_BOUND ( 'NONE', #15667, .T. ) ;
#4018 = DIRECTION ( 'NONE',  ( -1.000000000000000000, 0.000000000000000000, -0.000000000000000000 ) ) ;
#4019 = AXIS2_PLACEMENT_3D ( 'NONE', #8589, #5913, #10119 ) ;
#4020 = VECTOR ( 'NONE', #6754, 1000.000000000000000 ) ;
#4021 = DIRECTION ( 'NONE',  ( -1.000000000000000000, 0.000000000000000000, 0.000000000000000000 ) ) ;
#4022 = DIRECTION ( 'NONE',  ( 0.000000000000000000, 0.000000000000000000, 1.000000000000000000 ) ) ;
#4023 = EDGE_CURVE ( 'NONE', #6557, #1864, #9020, .T. ) ;
#4024 = CONTEXT_DEPENDENT_SHAPE_REPRESENTATION ( #17538, #12259 ) ;
#4025 = ADVANCED_FACE ( 'NONE', ( #14928 ), #10538, .F. ) ;
#4026 = VERTEX_POINT ( 'NONE', #17970 ) ;
#4027 = B_SPLINE_CURVE_WITH_KNOTS ( 'NONE', 3,
 ( #17495, #6062, #4633, #14638, #2750, #15799, #3117, #10353 ),
 .UNSPECIFIED., .F., .F.,
 ( 4, 2, 2, 4 ),
 ( 0.000000000000000000, 0.002450665683189819262, 0.003675998524784728893, 0.004901331366379639391 ),
 .UNSPECIFIED. ) ;
#4028 = EDGE_CURVE ( 'NONE', #13569, #12768, #3495, .T. ) ;
#4029 = ORIENTED_EDGE ( 'NONE', *, *, #11169, .T. ) ;
#4030 = ADVANCED_FACE ( 'NONE', ( #13314 ), #14731, .T. ) ;
#4031 = ORIENTED_EDGE ( 'NONE', *, *, #7053, .F. ) ;
#4033 = DIRECTION ( 'NONE',  ( -1.000000000000000000, -0.000000000000000000, -0.000000000000000000 ) ) ;
#4032 = VECTOR ( 'NONE', #1427, 1000.000000000000000 ) ;
#4034 = CARTESIAN_POINT ( 'NONE',  ( -90.00000000009001155, 1.000000000000014655, 5.000000000000003553 ) ) ;
#4035 = CARTESIAN_POINT ( 'NONE',  ( 50.00005079999999680, 0.000000000000000000, 30.00000000000000000 ) ) ;
#4036 = CARTESIAN_POINT ( 'NONE',  ( 10.00000000000000000, -5.940243314903991489, -32.46095361140698543 ) ) ;
#4037 = CARTESIAN_POINT ( 'NONE',  ( -90.40196296004810961, -14.11572627500821042, 6.951864913735147589 ) ) ;
#4038 = CARTESIAN_POINT ( 'NONE',  ( 10.00000000000000000, 0.000000000000000000, 0.000000000000000000 ) ) ;
#4039 = DIRECTION ( 'NONE',  ( 0.000000000000000000, 0.000000000000000000, 1.000000000000000000 ) ) ;
#4040 = EDGE_LOOP ( 'NONE', ( #5014, #3118, #16213, #8341, #14044 ) ) ;
#4041 = CARTESIAN_POINT ( 'NONE',  ( 0.000000000000000000, -46.20417134726108088, -32.31183295104820985 ) ) ;
#4042 = VERTEX_POINT ( 'NONE', #1682 ) ;
#4043 = PRODUCT ( 'socket head cap screw_iso_ISO 4762 M5 x 16 - 16N', 'socket head cap screw_iso_ISO 4762 M5 x 16 - 16N', '', ( #17185 ) ) ;
#4044 = DIRECTION ( 'NONE',  ( 0.000000000000000000, 0.000000000000000000, 1.000000000000000000 ) ) ;
#4045 = CARTESIAN_POINT ( 'NONE',  ( 45.00000000000000000, 0.000000000000000000, -5.120903701083534543E-13 ) ) ;
#4046 = ORIENTED_EDGE ( 'NONE', *, *, #10927, .F. ) ;
#4047 = DIRECTION ( 'NONE',  ( 0.000000000000000000, -1.000000000000000000, 0.000000000000000000 ) ) ;
#4048 = CARTESIAN_POINT ( 'NONE',  ( -26.29305231718568336, -39.99999999999999289, -19.10302069950552095 ) ) ;
#4049 = AXIS2_PLACEMENT_3D ( 'NONE', #2956, #8750, #14568 ) ;
#4050 = CARTESIAN_POINT ( 'NONE',  ( 10.00000000000000000, 20.32630374611185786, 16.60877409751175904 ) ) ;
#4051 = ORIENTED_EDGE ( 'NONE', *, *, #18226, .T. ) ;
#4052 = EDGE_CURVE ( 'NONE', #9572, #6420, #549, .T. ) ;
#4053 = CARTESIAN_POINT ( 'NONE',  ( 0.000000000000000000, 0.000000000000000000, 0.000000000000000000 ) ) ;
#4054 = CARTESIAN_POINT ( 'NONE',  ( 10.00000000000000000, 0.000000000000000000, 0.000000000000000000 ) ) ;
#4055 = DIRECTION ( 'NONE',  ( 0.000000000000000000, 1.000000000000000000, 3.491481338843133355E-15 ) ) ;
#4056 = CARTESIAN_POINT ( 'NONE',  ( -117.1020693116506379, -34.99999999999999289, -17.04080595179801705 ) ) ;
#4057 = AXIS2_PLACEMENT_3D ( 'NONE', #4062, #5491, #2622 ) ;
#4058 = AXIS2_PLACEMENT_3D ( 'NONE', #11343, #9822, #18589 ) ;
#4059 = CARTESIAN_POINT ( 'NONE',  ( 10.00000000000000000, 16.60877409751168443, 20.32630374611190405 ) ) ;
#4060 = VERTEX_POINT ( 'NONE', #16359 ) ;
#4061 = DIRECTION ( 'NONE',  ( 0.000000000000000000, 0.7071067811865485719, -0.7071067811865463515 ) ) ;
#4062 = CARTESIAN_POINT ( 'NONE',  ( 10.00000000000000000, 0.000000000000000000, 0.000000000000000000 ) ) ;
#4063 = DIRECTION ( 'NONE',  ( -1.000000000000000000, 0.000000000000000000, -0.000000000000000000 ) ) ;
#4064 = ORIENTED_EDGE ( 'NONE', *, *, #966, .T. ) ;
#4065 = VERTEX_POINT ( 'NONE', #10441 ) ;
#4066 = CARTESIAN_POINT ( 'NONE',  ( -17.77999999999999758, 3.673940397442059967E-15, -30.00000000000000711 ) ) ;
#4067 = EDGE_CURVE ( 'NONE', #4463, #13753, #7164, .T. ) ;
#4068 = VERTEX_POINT ( 'NONE', #6157 ) ;
#4069 = DIRECTION ( 'NONE',  ( 0.000000000000000000, 0.8910065241883688980, -0.4539904997395446951 ) ) ;
#4070 = EDGE_CURVE ( 'NONE', #4975, #6521, #9290, .T. ) ;
#4071 = DIRECTION ( 'NONE',  ( -1.000000000000000000, -0.000000000000000000, -0.000000000000000000 ) ) ;
#4072 = CARTESIAN_POINT ( 'NONE',  ( 10.04305231718605285, -26.50000000000000000, -33.55933677959240669 ) ) ;
#4073 = EDGE_LOOP ( 'NONE', ( #11865, #9142, #15557, #1248 ) ) ;
#4074 = CARTESIAN_POINT ( 'NONE',  ( -23.50000000000000355, 2.877919977996280715E-15, -2.000000000000000000 ) ) ;
#4075 = VERTEX_POINT ( 'NONE', #355 ) ;
#4076 = DIRECTION ( 'NONE',  ( -0.000000000000000000, 1.000000000000000000, -0.000000000000000000 ) ) ;
#4077 = DIRECTION ( 'NONE',  ( 0.000000000000000000, 0.000000000000000000, -1.000000000000000000 ) ) ;
#4078 = CARTESIAN_POINT ( 'NONE',  ( 10.00000000000000000, 0.000000000000000000, 0.000000000000000000 ) ) ;
#4079 = ORIENTED_EDGE ( 'NONE', *, *, #4757, .T. ) ;
#4080 = CARTESIAN_POINT ( 'NONE',  ( 0.000000000000000000, -34.99999999999999289, 0.000000000000000000 ) ) ;
#4081 = EDGE_LOOP ( 'NONE', ( #4782, #10644, #2067, #3925 ) ) ;
#4082 = LINE ( 'NONE', #1319, #1494 ) ;
#4083 = DIRECTION ( 'NONE',  ( 1.000000000000000000, 0.000000000000000000, -0.000000000000000000 ) ) ;
#4084 = VERTEX_POINT ( 'NONE', #7765 ) ;
#4085 = ORIENTED_EDGE ( 'NONE', *, *, #16122, .T. ) ;
#4086 = EDGE_CURVE ( 'NONE', #9292, #18350, #10516, .T. ) ;
#4087 = CARTESIAN_POINT ( 'NONE',  ( 10.00000000000000000, -20.41355805489602204, -19.44239304137396118 ) ) ;
#4088 =( NAMED_UNIT ( * ) SI_UNIT ( $, .STERADIAN. ) SOLID_ANGLE_UNIT ( ) );
#4089 = EDGE_CURVE ( 'NONE', #10426, #3123, #3213, .T. ) ;
#4090 = ORIENTED_EDGE ( 'NONE', *, *, #10079, .F. ) ;
#4091 = CARTESIAN_POINT ( 'NONE',  ( -3.999999999999999112, -2.309401076758512694, -3.504269196027871125 ) ) ;
#4092 = CARTESIAN_POINT ( 'NONE',  ( 2.500000000000000000, -1.178949249685218748, -2.041999999999998039 ) ) ;
#4093 = EDGE_CURVE ( 'NONE', #18122, #4173, #10214, .T. ) ;
#4094 = VERTEX_POINT ( 'NONE', #17773 ) ;
#4095 = EDGE_LOOP ( 'NONE', ( #3065, #4196, #12387, #7301 ) ) ;
#4096 = FACE_OUTER_BOUND ( 'NONE', #14033, .T. ) ;
#4097 = DIRECTION ( 'NONE',  ( -0.000000000000000000, -0.000000000000000000, 1.000000000000000000 ) ) ;
#4098 = CARTESIAN_POINT ( 'NONE',  ( 11.25000000000000000, 0.000000000000000000, 0.000000000000000000 ) ) ;
#4099 = DIRECTION ( 'NONE',  ( 0.000000000000000000, -0.8090169943749530024, 0.5877852522924653655 ) ) ;
#4100 = EDGE_CURVE ( 'NONE', #6721, #12768, #1390, .T. ) ;
#4101 = EDGE_CURVE ( 'NONE', #9667, #10550, #12969, .T. ) ;
#4102 = DIRECTION ( 'NONE',  ( -1.000000000000000000, 0.000000000000000000, 0.000000000000000000 ) ) ;
#4103 = DIRECTION ( 'NONE',  ( -1.000000000000000000, 0.000000000000000000, -0.000000000000000000 ) ) ;
#4104 = CARTESIAN_POINT ( 'NONE',  ( 4.999999999999999112, 57.83923611457355918, -24.97244012287440285 ) ) ;
#4105 = ORIENTED_EDGE ( 'NONE', *, *, #11525, .T. ) ;
#4106 = CYLINDRICAL_SURFACE ( 'NONE', #13374, 12.00000000001200107 ) ;
#4107 = DIRECTION ( 'NONE',  ( -1.000000000000000000, -0.000000000000000000, -0.000000000000000000 ) ) ;
#4108 = DIRECTION ( 'NONE',  ( -1.000000000000000000, -0.000000000000000000, 0.000000000000000000 ) ) ;
#4109 = DIRECTION ( 'NONE',  ( 0.000000000000000000, 0.000000000000000000, 1.000000000000000000 ) ) ;
#4110 = CIRCLE ( 'NONE', #14131, 20.00000000000000000 ) ;
#4111 = ORIENTED_EDGE ( 'NONE', *, *, #6339, .T. ) ;
#4112 = ADVANCED_FACE ( 'NONE', ( #3975, #9574 ), #932, .F. ) ;
#4113 = VERTEX_POINT ( 'NONE', #16828 ) ;
#4114 = DIRECTION ( 'NONE',  ( -1.000000000000000000, -0.000000000000000000, 0.000000000000000000 ) ) ;
#4115 = DIRECTION ( 'NONE',  ( 0.000000000000000000, 0.000000000000000000, -1.000000000000000000 ) ) ;
#4116 = DIRECTION ( 'NONE',  ( 0.000000000000000000, 0.000000000000000000, 1.000000000000000000 ) ) ;
#4117 = CIRCLE ( 'NONE', #13844, 63.00000000006298961 ) ;
#4118 = ORIENTED_EDGE ( 'NONE', *, *, #12722, .T. ) ;
#4119 = FILL_AREA_STYLE ('',( #17172 ) ) ;
#4120 = AXIS2_PLACEMENT_3D ( 'NONE', #18310, #11060, #16887 ) ;
#4121 = DIRECTION ( 'NONE',  ( 1.000000000000000000, 0.000000000000000000, 0.000000000000000000 ) ) ;
#4122 = EDGE_CURVE ( 'NONE', #3732, #8023, #8257, .T. ) ;
#4123 = EDGE_CURVE ( 'NONE', #13348, #11649, #6817, .T. ) ;
#4124 = EDGE_CURVE ( 'NONE', #6225, #15269, #15372, .T. ) ;
#4125 = CARTESIAN_POINT ( 'NONE',  ( 0.000000000000000000, 13.24999999999999467, 0.000000000000000000 ) ) ;
#4126 = DIRECTION ( 'NONE',  ( 0.000000000000000000, 0.000000000000000000, -1.000000000000000000 ) ) ;
#4127 = DIRECTION ( 'NONE',  ( 0.000000000000000000, 0.000000000000000000, 1.000000000000000000 ) ) ;
#4128 = EDGE_LOOP ( 'NONE', ( #15888, #11696, #18574, #9456, #462, #10346, #9599, #11708, #5405, #18054, #3591, #5471, #3111, #15508, #7966, #15270, #82, #3329, #6344, #3119, #16119, #3254, #13926, #13969, #5747, #4373, #18369, #11733, #5891, #710, #3400, #5852, #14972, #18316, #18028, #11470, #716, #13918, #14413, #8028, #10248, #5289, #9158, #16996, #12047, #9560, #18801, #12225, #954, #13815, #2186, #10955, #18046, #5002, #14930, #16259, #12601, #14020, #17803, #11601, #10508, #3469, #4004, #2217, #11398, #14035, #18231, #2826, #15899, #3747, #2092, #15389, #15747, #9300, #5219, #16826, #259, #14356, #1419, #17388, #7042, #5597, #6019, #3245, #8321 ) ) ;
#4129 = CARTESIAN_POINT ( 'NONE',  ( -4.000000000000000000, 0.000000000000000000, 0.000000000000000000 ) ) ;
#4130 = ORIENTED_EDGE ( 'NONE', *, *, #5680, .F. ) ;
#4131 = EDGE_CURVE ( 'NONE', #8705, #8908, #11437, .T. ) ;
#4132 = CARTESIAN_POINT ( 'NONE',  ( 5.000000000000000000, -14.27431201565505425, -29.75305054077487199 ) ) ;
#4133 = DIRECTION ( 'NONE',  ( -1.000000000000000000, 0.000000000000000000, 0.000000000000000000 ) ) ;
#4134 = ORIENTED_EDGE ( 'NONE', *, *, #16131, .F. ) ;
#4135 = PRESENTATION_LAYER_ASSIGNMENT (  '', '', ( #10838 ) ) ;
#4136 = EDGE_CURVE ( 'NONE', #12242, #6225, #12338, .T. ) ;
#4137 = DIRECTION ( 'NONE',  ( -1.000000000000000000, -0.000000000000000000, 0.000000000000000000 ) ) ;
#4138 = SHAPE_DEFINITION_REPRESENTATION ( #7701, #16765 ) ;
#4139 = CYLINDRICAL_SURFACE ( 'NONE', #12376, 63.00000000006298961 ) ;
#4140 = ORIENTED_EDGE ( 'NONE', *, *, #865, .T. ) ;
#4141 = VECTOR ( 'NONE', #4621, 999.9999999999998863 ) ;
#4142 = CIRCLE ( 'NONE', #1093, 24.00000000002400213 ) ;
#4143 = EDGE_CURVE ( 'NONE', #6887, #17793, #8989, .T. ) ;
#4144 = CARTESIAN_POINT ( 'NONE',  ( 0.000000000000000000, 4.007856633823394077, 62.87238730325622527 ) ) ;
#4145 = LINE ( 'NONE', #14241, #3654 ) ;
#4146 = VECTOR ( 'NONE', #3470, 1000.000000000000000 ) ;
#4147 = DIRECTION ( 'NONE',  ( 0.000000000000000000, 0.000000000000000000, -1.000000000000000000 ) ) ;
#4148 = CARTESIAN_POINT ( 'NONE',  ( 5.032868406504335645, -28.36021363089093938, -2.000000000000000000 ) ) ;
#4149 = EDGE_CURVE ( 'NONE', #11786, #14902, #1690, .T. ) ;
#4150 = CIRCLE ( 'NONE', #7475, 56.24900000005625600 ) ;
#4151 = AXIS2_PLACEMENT_3D ( 'NONE', #2437, #15114, #11087 ) ;
#4152 = CARTESIAN_POINT ( 'NONE',  ( 0.000000000000000000, 6.681932690256967788, 25.38428207620324883 ) ) ;
#4153 = AXIS2_PLACEMENT_3D ( 'NONE', #6766, #1342, #8388 ) ;
#4154 = EDGE_LOOP ( 'NONE', ( #7724, #2376 ) ) ;
#4155 = DIRECTION ( 'NONE',  ( 0.000000000000000000, 0.7071067811865485719, -0.7071067811865463515 ) ) ;
#4156 = DIRECTION ( 'NONE',  ( 0.000000000000000000, 0.4539904997395479147, -0.8910065241883673437 ) ) ;
#4157 = CARTESIAN_POINT ( 'NONE',  ( 0.000000000000000000, -17.25000000000000355, 0.000000000000000000 ) ) ;
#4158 = VERTEX_POINT ( 'NONE', #6914 ) ;
#4159 = ORIENTED_EDGE ( 'NONE', *, *, #11695, .F. ) ;
#4160 = EDGE_CURVE ( 'NONE', #2985, #11786, #14457, .T. ) ;
#4161 = CARTESIAN_POINT ( 'NONE',  ( 2.500000000000000000, -1.178949249685214307, 2.042000000000001592 ) ) ;
#4162 = ORIENTED_EDGE ( 'NONE', *, *, #3137, .T. ) ;
#4163 = FACE_OUTER_BOUND ( 'NONE', #10157, .T. ) ;
#4164 = CIRCLE ( 'NONE', #5354, 56.24900000005625600 ) ;
#4165 = AXIS2_PLACEMENT_3D ( 'NONE', #15259, #8013, #14025 ) ;
#4166 = CIRCLE ( 'NONE', #17236, 24.00000000002399858 ) ;
#4167 = CARTESIAN_POINT ( 'NONE',  ( 0.000000000000000000, 0.000000000000000000, -1.000000000000000000 ) ) ;
#4168 = DIRECTION ( 'NONE',  ( 0.000000000000000000, 1.000000000000000000, -1.287488025362403787E-15 ) ) ;
#4169 =( REPRESENTATION_RELATIONSHIP ('NONE','NONE', #11014, #2517 ) REPRESENTATION_RELATIONSHIP_WITH_TRANSFORMATION ( #12489 )SHAPE_REPRESENTATION_RELATIONSHIP( ) );
#4170 = VERTEX_POINT ( 'NONE', #18055 ) ;
#4171 = DIRECTION ( 'NONE',  ( 0.000000000000000000, 0.000000000000000000, 1.000000000000000000 ) ) ;
#4172 = CIRCLE ( 'NONE', #502, 41.00000000000000000 ) ;
#4173 = VERTEX_POINT ( 'NONE', #1020 ) ;
#4175 = AXIS2_PLACEMENT_3D ( 'NONE', #10080, #14364, #4448 ) ;
#4174 = PLANE ( 'NONE',  #2674 ) ;
#4176 = ORIENTED_EDGE ( 'NONE', *, *, #2980, .T. ) ;
#4177 = DIRECTION ( 'NONE',  ( 0.000000000000000000, 0.000000000000000000, 1.000000000000000000 ) ) ;
#4178 = VERTEX_POINT ( 'NONE', #11200 ) ;
#4179 = AXIS2_PLACEMENT_3D ( 'NONE', #18479, #12480, #18285 ) ;
#4180 = DIRECTION ( 'NONE',  ( 0.000000000000000000, 0.000000000000000000, 1.000000000000000000 ) ) ;
#4181 = DIRECTION ( 'NONE',  ( -1.000000000000000000, 0.000000000000000000, 0.000000000000000000 ) ) ;
#4182 = CIRCLE ( 'NONE', #13293, 23.50000000000000355 ) ;
#4183 = ORIENTED_EDGE ( 'NONE', *, *, #824, .T. ) ;
#4184 = EDGE_LOOP ( 'NONE', ( #18752, #7134, #1587, #7545 ) ) ;
#4185 = EDGE_CURVE ( 'NONE', #9008, #13142, #2612, .T. ) ;
#4186 = DIRECTION ( 'NONE',  ( 1.000000000000000000, 0.000000000000000000, 0.000000000000000000 ) ) ;
#4187 = ORIENTED_EDGE ( 'NONE', *, *, #2620, .T. ) ;
#4188 = CARTESIAN_POINT ( 'NONE',  ( 4.999999999999999112, 4.381479206523446912, -32.70783759231082399 ) ) ;
#4189 = CARTESIAN_POINT ( 'NONE',  ( 10.00000000000000000, 49.49802920186223076, 26.71881558261748069 ) ) ;
#4190 = CIRCLE ( 'NONE', #6616, 0.7500000000000000000 ) ;
#4191 = VECTOR ( 'NONE', #16551, 1000.000000000000000 ) ;
#4192 = CYLINDRICAL_SURFACE ( 'NONE', #374, 25.00000000000000000 ) ;
#4193 = VECTOR ( 'NONE', #7476, 1000.000000000000000 ) ;
#4194 = CIRCLE ( 'NONE', #6619, 25.10000000000000142 ) ;
#4195 = ADVANCED_FACE ( 'NONE', ( #3598 ), #12628, .T. ) ;
#4196 = ORIENTED_EDGE ( 'NONE', *, *, #14850, .F. ) ;
#4197 = EDGE_LOOP ( 'NONE', ( #15144, #13402 ) ) ;
#4198 = CARTESIAN_POINT ( 'NONE',  ( -36.40576474687247099, 10.00000000000000000, 29.10033635316149514 ) ) ;
#4199 = DIRECTION ( 'NONE',  ( 0.000000000000000000, 1.000000000000000000, 0.000000000000000000 ) ) ;
#4200 = DIRECTION ( 'NONE',  ( 0.000000000000000000, 0.000000000000000000, 1.000000000000000000 ) ) ;
#4201 = FACE_OUTER_BOUND ( 'NONE', #6624, .T. ) ;
#4202 = EDGE_CURVE ( 'NONE', #16450, #15559, #15696, .T. ) ;
#4203 = CARTESIAN_POINT ( 'NONE',  ( 10.00000000000000000, -3.730438010304518492, 27.94286728106391138 ) ) ;
#4204 = DIRECTION ( 'NONE',  ( 0.000000000000000000, 0.000000000000000000, 1.000000000000000000 ) ) ;
#4205 = AXIS2_PLACEMENT_3D ( 'NONE', #7482, #3394, #436 ) ;
#4206 = FACE_OUTER_BOUND ( 'NONE', #12915, .T. ) ;
#4207 = VERTEX_POINT ( 'NONE', #15494 ) ;
#4208 = CARTESIAN_POINT ( 'NONE',  ( 10.00000000000000000, 55.51919907100653973, 9.823366686500859757 ) ) ;
#4209 = DIRECTION ( 'NONE',  ( 1.000000000000000000, 0.000000000000000000, 0.000000000000000000 ) ) ;
#4210 = CARTESIAN_POINT ( 'NONE',  ( 0.000000000000000000, -23.24033432160398860, -58.55669782892485387 ) ) ;
#4211 = CARTESIAN_POINT ( 'NONE',  ( 5.000000000000000000, -33.71303790549235657, -53.22058882792234158 ) ) ;
#4212 = CIRCLE ( 'NONE', #14842, 63.00000000006298961 ) ;
#4213 = ORIENTED_EDGE ( 'NONE', *, *, #18657, .T. ) ;
#4214 = AXIS2_PLACEMENT_3D ( 'NONE', #18532, #17300, #5576 ) ;
#4215 = EDGE_LOOP ( 'NONE', ( #8073, #13068, #14235, #14500 ) ) ;
#4216 = AXIS2_PLACEMENT_3D ( 'NONE', #11563, #4133, #5475 ) ;
#4217 = CARTESIAN_POINT ( 'NONE',  ( 10.00000000000000000, 0.000000000000000000, 0.000000000000000000 ) ) ;
#4218 = DIRECTION ( 'NONE',  ( 1.000000000000000000, -0.000000000000000000, -0.000000000000000000 ) ) ;
#4219 = COLOUR_RGB ( '',1.000000000000000000, 0.9490196078431372140, 0.9098039215686274384 ) ;
#4220 = ORIENTED_EDGE ( 'NONE', *, *, #17207, .T. ) ;
#4221 = CIRCLE ( 'NONE', #18807, 63.00000000006298961 ) ;
#4222 =( LENGTH_UNIT ( ) NAMED_UNIT ( * ) SI_UNIT ( .MILLI., .METRE. ) );
#4223 = CYLINDRICAL_SURFACE ( 'NONE', #14188, 24.00000000002399858 ) ;
#4224 = DIRECTION ( 'NONE',  ( -1.000000000000000000, -0.000000000000000000, -0.000000000000000000 ) ) ;
#4225 = LINE ( 'NONE', #4496, #6137 ) ;
#4226 = CARTESIAN_POINT ( 'NONE',  ( 10.00000000000000000, -27.94286728106395756, 15.73043801031622912 ) ) ;
#4227 = ADVANCED_BREP_SHAPE_REPRESENTATION ( '', ( #9242, #8017 ), #1061 ) ;
#4228 = ORIENTED_EDGE ( 'NONE', *, *, #15943, .T. ) ;
#4229 = CARTESIAN_POINT ( 'NONE',  ( 10.00000000000000000, -31.97297851452390915, -46.27827401617439307 ) ) ;
#4230 = VERTEX_POINT ( 'NONE', #2443 ) ;
#4231 = CARTESIAN_POINT ( 'NONE',  ( 0.000000000000000000, -16.60877409751153522, -20.32630374611203194 ) ) ;
#4232 = DIRECTION ( 'NONE',  ( 0.000000000000000000, 0.000000000000000000, -1.000000000000000000 ) ) ;
#4233 = ORIENTED_EDGE ( 'NONE', *, *, #6890, .F. ) ;
#4234 = PRODUCT_CONTEXT ( 'NONE', #16684, 'mechanical' ) ;
#4235 = AXIS2_PLACEMENT_3D ( 'NONE', #9037, #1810, #11898 ) ;
#4236 = DIRECTION ( 'NONE',  ( 0.000000000000000000, 0.000000000000000000, 1.000000000000000000 ) ) ;
#4237 = ORIENTED_EDGE ( 'NONE', *, *, #10084, .F. ) ;
#4238 = CIRCLE ( 'NONE', #9086, 56.24900000005625600 ) ;
#4239 = CIRCLE ( 'NONE', #15172, 33.00000000003299760 ) ;
#4240 = EDGE_CURVE ( 'NONE', #8632, #5801, #5661, .T. ) ;
#4241 = EDGE_CURVE ( 'NONE', #4178, #2244, #13560, .T. ) ;
#4242 = ADVANCED_FACE ( 'NONE', ( #18153 ), #2245, .T. ) ;
#4243 = ORIENTED_EDGE ( 'NONE', *, *, #10832, .F. ) ;
#4244 = CARTESIAN_POINT ( 'NONE',  ( 0.000000000000000000, 3.673940397442059178E-15, -30.00000000000000000 ) ) ;
#4245 = EDGE_CURVE ( 'NONE', #7186, #7123, #16903, .T. ) ;
#4246 = DIRECTION ( 'NONE',  ( 0.000000000000000000, 1.000000000000000000, 0.000000000000000000 ) ) ;
#4247 = CIRCLE ( 'NONE', #3628, 33.00000000003299760 ) ;
#4248 = DIRECTION ( 'NONE',  ( -1.000000000000000000, -0.000000000000000000, 0.000000000000000000 ) ) ;
#4249 = LINE ( 'NONE', #11577, #17990 ) ;
#4250 = VECTOR ( 'NONE', #2249, 1000.000000000000000 ) ;
#4251 = EDGE_CURVE ( 'NONE', #8328, #13117, #1302, .T. ) ;
#4252 = DIRECTION ( 'NONE',  ( -1.000000000000000000, 0.000000000000000000, 0.000000000000000000 ) ) ;
#4253 = ORIENTED_EDGE ( 'NONE', *, *, #5918, .T. ) ;
#4254 = FACE_OUTER_BOUND ( 'NONE', #8728, .T. ) ;
#4255 = ADVANCED_FACE ( 'NONE', ( #5583 ), #11671, .T. ) ;
#4256 = CARTESIAN_POINT ( 'NONE',  ( 2.500000000000000000, -1.178949249685213863, 2.042000000000001148 ) ) ;
#4257 = DIRECTION ( 'NONE',  ( -1.000000000000000000, 0.000000000000000000, 0.000000000000000000 ) ) ;
#4258 = ORIENTED_EDGE ( 'NONE', *, *, #5027, .T. ) ;
#4259 = ORIENTED_EDGE ( 'NONE', *, *, #531, .F. ) ;
#4260 = CARTESIAN_POINT ( 'NONE',  ( 10.00000000000000000, 54.20017844242511273, 32.11449294037215196 ) ) ;
#4261 =( LENGTH_UNIT ( ) NAMED_UNIT ( * ) SI_UNIT ( .MILLI., .METRE. ) );
#4262 = ORIENTED_EDGE ( 'NONE', *, *, #6787, .F. ) ;
#4263 = EDGE_CURVE ( 'NONE', #14803, #8173, #1100, .T. ) ;
#4264 = CARTESIAN_POINT ( 'NONE',  ( 10.00000000000000000, 32.70783759231085952, -4.381479206523099634 ) ) ;
#4265 = LINE ( 'NONE', #17401, #9966 ) ;
#4266 = EDGE_CURVE ( 'NONE', #912, #11392, #14623, .T. ) ;
#4267 = VERTEX_POINT ( 'NONE', #7011 ) ;
#4268 = CARTESIAN_POINT ( 'NONE',  ( 0.000000000000000000, 0.000000000000000000, 0.000000000000000000 ) ) ;
#4269 = AXIS2_PLACEMENT_3D ( 'NONE', #15776, #17571, #14250 ) ;
#4270 = VERTEX_POINT ( 'NONE', #1488 ) ;
#4271 = FACE_BOUND ( 'NONE', #580, .T. ) ;
#4272 = VERTEX_POINT ( 'NONE', #17311 ) ;
#4273 = CARTESIAN_POINT ( 'NONE',  ( 0.000000000000000000, 14.27431201565524788, 29.75305054077477607 ) ) ;
#4274 = ORIENTED_EDGE ( 'NONE', *, *, #8429, .T. ) ;
#4275 = AXIS2_PLACEMENT_3D ( 'NONE', #8430, #12612, #2714 ) ;
#4276 = DIRECTION ( 'NONE',  ( -1.000000000000000000, -0.000000000000000000, -0.000000000000000000 ) ) ;
#4277 = CARTESIAN_POINT ( 'NONE',  ( -0.1481481481481481122, -4.797713218419819903, -1.000000000000000000 ) ) ;
#4278 = ORIENTED_EDGE ( 'NONE', *, *, #14611, .T. ) ;
#4279 = ORIENTED_EDGE ( 'NONE', *, *, #15124, .F. ) ;
#4280 = DIRECTION ( 'NONE',  ( 0.000000000000000000, 0.000000000000000000, 1.000000000000000000 ) ) ;
#4281 = ORIENTED_EDGE ( 'NONE', *, *, #12573, .F. ) ;
#4282 = CARTESIAN_POINT ( 'NONE',  ( 10.00000000000000000, -46.27827401617379621, -31.97297851452475470 ) ) ;
#4283 = APPLICATION_CONTEXT ( 'automotive_design' ) ;
#4284 = PRESENTATION_LAYER_ASSIGNMENT (  '', '', ( #16446 ) ) ;
#4285 = DIRECTION ( 'NONE',  ( -1.000000000000000000, 0.000000000000000000, -0.000000000000000000 ) ) ;
#4286 = EDGE_CURVE ( 'NONE', #701, #13284, #15081, .T. ) ;
#4287 = ORIENTED_EDGE ( 'NONE', *, *, #1104, .F. ) ;
#4288 = ORIENTED_EDGE ( 'NONE', *, *, #13070, .F. ) ;
#4289 = CARTESIAN_POINT ( 'NONE',  ( 10.00000000000000000, 26.71881558261799228, -49.49802920186195365 ) ) ;
#4290 = CYLINDRICAL_SURFACE ( 'NONE', #12929, 12.00000000001200462 ) ;
#4291 = CARTESIAN_POINT ( 'NONE',  ( 0.000000000000000000, 0.000000000000000000, 0.000000000000000000 ) ) ;
#4292 = CARTESIAN_POINT ( 'NONE',  ( 2.500000000000000000, -1.178949249685213863, 2.042000000000001148 ) ) ;
#4293 = CARTESIAN_POINT ( 'NONE',  ( 2.500000000000000000, -2.357898499370431722, 2.818925648462311528E-15 ) ) ;
#4294 = CYLINDRICAL_SURFACE ( 'NONE', #3427, 24.00000000002399503 ) ;
#4295 = LINE ( 'NONE', #16095, #1413 ) ;
#4296 = ORIENTED_EDGE ( 'NONE', *, *, #9114, .T. ) ;
#4297 = DIRECTION ( 'NONE',  ( -1.000000000000000000, 0.000000000000000000, 0.000000000000000000 ) ) ;
#4298 = CIRCLE ( 'NONE', #14934, 63.00000000006298961 ) ;
#4299 = CARTESIAN_POINT ( 'NONE',  ( 10.00000000000000000, 5.086963483077590276, -27.72801475327276677 ) ) ;
#4300 = ORIENTED_EDGE ( 'NONE', *, *, #13770, .F. ) ;
#4301 = LINE ( 'NONE', #7139, #6037 ) ;
#4302 = LINE ( 'NONE', #3058, #2823 ) ;
#4303 = EDGE_CURVE ( 'NONE', #2260, #2267, #7470, .T. ) ;
#4304 = ORIENTED_EDGE ( 'NONE', *, *, #272, .F. ) ;
#4305 = EDGE_CURVE ( 'NONE', #4564, #9997, #14428, .T. ) ;
#4306 = ORIENTED_EDGE ( 'NONE', *, *, #1296, .F. ) ;
#4307 = AXIS2_PLACEMENT_3D ( 'NONE', #6520, #3678, #12327 ) ;
#4308 = DIRECTION ( 'NONE',  ( 0.000000000000000000, 0.000000000000000000, -1.000000000000000000 ) ) ;
#4309 = CARTESIAN_POINT ( 'NONE',  ( 10.00000000000000000, -53.06836994729219725, -18.64666490672428623 ) ) ;
#4310 = ORIENTED_EDGE ( 'NONE', *, *, #3220, .T. ) ;
#4311 = DIRECTION ( 'NONE',  ( -1.000000000000000000, -0.000000000000000000, 0.000000000000000000 ) ) ;
#4312 = CARTESIAN_POINT ( 'NONE',  ( 0.000000000000000000, 0.000000000000000000, 0.000000000000000000 ) ) ;
#4313 = CIRCLE ( 'NONE', #6737, 150.0000000000000284 ) ;
#4314 = DIRECTION ( 'NONE',  ( -1.000000000000000000, 0.000000000000000000, 0.000000000000000000 ) ) ;
#4315 = CARTESIAN_POINT ( 'NONE',  ( 0.000000000000000000, 0.000000000000000000, 0.000000000000000000 ) ) ;
#4316 = LINE ( 'NONE', #8505, #8391 ) ;
#4317 = VERTEX_POINT ( 'NONE', #4260 ) ;
#4318 = CARTESIAN_POINT ( 'NONE',  ( 4.999999999999997335, 0.000000000000000000, 0.000000000000000000 ) ) ;
#4319 = VERTEX_POINT ( 'NONE', #5777 ) ;
#4320 = CARTESIAN_POINT ( 'NONE',  ( 10.00000000000000000, 0.000000000000000000, 0.000000000000000000 ) ) ;
#4321 = CARTESIAN_POINT ( 'NONE',  ( -79.64793068852898728, -30.00000000000000000, -34.51039329588756033 ) ) ;
#4322 = ORIENTED_EDGE ( 'NONE', *, *, #4470, .F. ) ;
#4323 = PRODUCT_CONTEXT ( 'NONE', #10463, 'mechanical' ) ;
#4324 = ORIENTED_EDGE ( 'NONE', *, *, #11471, .T. ) ;
#4325 = CIRCLE ( 'NONE', #15894, 2.649999999999999467 ) ;
#4326 = CARTESIAN_POINT ( 'NONE',  ( 0.000000000000000000, -26.49895292618039377, 49.76630880786299826 ) ) ;
#4327 = DIRECTION ( 'NONE',  ( -1.000000000000000000, 0.000000000000000000, 0.000000000000000000 ) ) ;
#4328 = CARTESIAN_POINT ( 'NONE',  ( 0.1481481481481481122, -4.797713218419819903, 0.000000000000000000 ) ) ;
#4329 = DIRECTION ( 'NONE',  ( 0.000000000000000000, -6.982962677686266711E-15, 1.000000000000000000 ) ) ;
#4330 = CIRCLE ( 'NONE', #6757, 27.29487558977753991 ) ;
#4331 = DIRECTION ( 'NONE',  ( 0.000000000000000000, 0.000000000000000000, 1.000000000000000000 ) ) ;
#4332 = ORIENTED_EDGE ( 'NONE', *, *, #8841, .F. ) ;
#4333 = EDGE_CURVE ( 'NONE', #4919, #5529, #6864, .T. ) ;
#4334 = ADVANCED_FACE ( 'NONE', ( #10146 ), #17204, .F. ) ;
#4335 = DIRECTION ( 'NONE',  ( 0.000000000000000000, -0.8910065241883626808, -0.4539904997395568520 ) ) ;
#4336 = DIRECTION ( 'NONE',  ( 0.000000000000000000, 0.000000000000000000, 1.000000000000000000 ) ) ;
#4337 = CARTESIAN_POINT ( 'NONE',  ( 10.00000000000000000, 56.37237871411034007, 1.017308535512583711 ) ) ;
#4338 = ORIENTED_EDGE ( 'NONE', *, *, #2610, .F. ) ;
#4339 = ORIENTED_EDGE ( 'NONE', *, *, #10749, .F. ) ;
#4340 = DIRECTION ( 'NONE',  ( -1.000000000000000000, 0.000000000000000000, 0.000000000000000000 ) ) ;
#4341 = PRODUCT_RELATED_PRODUCT_CATEGORY ( 'part', '', ( #3293 ) ) ;
#4342 = ORIENTED_EDGE ( 'NONE', *, *, #12764, .T. ) ;
#4343 = ADVANCED_FACE ( 'NONE', ( #18628 ), #7188, .F. ) ;
#4344 = PRODUCT_DEFINITION_SHAPE ( 'NONE', 'NONE',  #18824 ) ;
#4345 = AXIS2_PLACEMENT_3D ( 'NONE', #3898, #18271, #2461 ) ;
#4346 = DIRECTION ( 'NONE',  ( -1.000000000000000000, 0.000000000000000000, 0.000000000000000000 ) ) ;
#4347 = CARTESIAN_POINT ( 'NONE',  ( 0.000000000000000000, 0.000000000000000000, 5.000000000000000000 ) ) ;
#4348 = ADVANCED_FACE ( 'NONE', ( #7291, #1575, #10057, #9865, #12825, #12730, #15954 ), #62, .F. ) ;
#4349 = AXIS2_PLACEMENT_3D ( 'NONE', #12020, #327, #4889 ) ;
#4350 = CLOSED_SHELL ( 'NONE', ( #6995, #13096, #15004, #17357, #3538, #17864, #17391, #16101, #2044, #16524, #18448, #16531, #2465, #15676, #16002, #10627, #1213, #2516, #16783, #16040, #13549, #6537 ) ) ;
#4351 = CARTESIAN_POINT ( 'NONE',  ( 0.000000000000000000, 24.46385708179984064, 9.514709542736980552 ) ) ;
#4352 = ORIENTED_EDGE ( 'NONE', *, *, #4665, .F. ) ;
#4353 = CARTESIAN_POINT ( 'NONE',  ( 0.000000000000000000, 0.000000000000000000, -1.000000000000000000 ) ) ;
#4354 = EDGE_LOOP ( 'NONE', ( #1855, #16404, #15887, #11580 ) ) ;
#4355 = FACE_OUTER_BOUND ( 'NONE', #10583, .T. ) ;
#4356 = VERTEX_POINT ( 'NONE', #5856 ) ;
#4358 = ORIENTED_EDGE ( 'NONE', *, *, #16168, .T. ) ;
#4357 = EDGE_CURVE ( 'NONE', #15093, #10166, #10238, .T. ) ;
#4359 = ADVANCED_FACE ( 'NONE', ( #15677 ), #8443, .T. ) ;
#4360 = CYLINDRICAL_SURFACE ( 'NONE', #12135, 2.649999999999999467 ) ;
#4361 = DIRECTION ( 'NONE',  ( 0.000000000000000000, 0.000000000000000000, 1.000000000000000000 ) ) ;
#4362 = EDGE_LOOP ( 'NONE', ( #3150, #9156 ) ) ;
#4363 = VERTEX_POINT ( 'NONE', #5495 ) ;
#4364 = CARTESIAN_POINT ( 'NONE',  ( 10.00000000000000000, 44.70888270294162226, 34.13306034420202906 ) ) ;
#4365 = EDGE_CURVE ( 'NONE', #12674, #9439, #5030, .T. ) ;
#4366 = ORIENTED_EDGE ( 'NONE', *, *, #9818, .F. ) ;
#4367 = CARTESIAN_POINT ( 'NONE',  ( 4.000000000000000000, 2.309401076758497151, -5.000000000000000000 ) ) ;
#4368 = AXIS2_PLACEMENT_3D ( 'NONE', #4755, #6278, #10837 ) ;
#4369 = EDGE_CURVE ( 'NONE', #11814, #3234, #7776, .T. ) ;
#4370 = DIRECTION ( 'NONE',  ( 0.000000000000000000, 0.000000000000000000, 1.000000000000000000 ) ) ;
#4371 = ORIENTED_EDGE ( 'NONE', *, *, #12808, .T. ) ;
#4372 = CIRCLE ( 'NONE', #5884, 4.799999999999998934 ) ;
#4373 = ORIENTED_EDGE ( 'NONE', *, *, #3526, .F. ) ;
#4374 = DIRECTION ( 'NONE',  ( -1.000000000000000000, 0.000000000000000000, -0.000000000000000000 ) ) ;
#4375 = LINE ( 'NONE', #10178, #10005 ) ;
#4376 = DIRECTION ( 'NONE',  ( -1.000000000000000000, -0.000000000000000000, 0.000000000000000000 ) ) ;
#4377 = CYLINDRICAL_SURFACE ( 'NONE', #10841, 30.39999999999999858 ) ;
#4378 = CARTESIAN_POINT ( 'NONE',  ( -4.000000000000000000, -0.8382240730041925492, -3.220610619767135141 ) ) ;
#4379 = CARTESIAN_POINT ( 'NONE',  ( 10.00000000000000000, -6.681932690257146312, 25.38428207620320620 ) ) ;
#4380 = DIRECTION ( 'NONE',  ( 0.000000000000000000, -1.000000000000000000, 0.000000000000000000 ) ) ;
#4381 = DIRECTION ( 'NONE',  ( 0.000000000000000000, 0.000000000000000000, 1.000000000000000000 ) ) ;
#4382 = ORIENTED_EDGE ( 'NONE', *, *, #8659, .T. ) ;
#4383 = DIRECTION ( 'NONE',  ( -1.000000000000000000, 0.000000000000000000, 0.000000000000000000 ) ) ;
#4384 = DIRECTION ( 'NONE',  ( -1.000000000000000000, -0.000000000000000000, -0.000000000000000000 ) ) ;
#4385 = VERTEX_POINT ( 'NONE', #13389 ) ;
#4386 = DIRECTION ( 'NONE',  ( -1.000000000000000000, -0.000000000000000000, 0.000000000000000000 ) ) ;
#4387 = CARTESIAN_POINT ( 'NONE',  ( 0.2500000000000002220, 0.000000000000000000, 4.250000000000000000 ) ) ;
#4388 = EDGE_CURVE ( 'NONE', #16102, #4891, #10093, .T. ) ;
#4389 = AXIS2_PLACEMENT_3D ( 'NONE', #18604, #8687, #10211 ) ;
#4390 = VERTEX_POINT ( 'NONE', #9090 ) ;
#4391 = CARTESIAN_POINT ( 'NONE',  ( 2.500000000000000000, 2.357898499370431722, -2.818925648462311528E-15 ) ) ;
#4392 = FACE_OUTER_BOUND ( 'NONE', #4549, .T. ) ;
#4393 = ORIENTED_EDGE ( 'NONE', *, *, #6732, .F. ) ;
#4394 = DIRECTION ( 'NONE',  ( 0.000000000000000000, -1.000000000000000000, 0.000000000000000000 ) ) ;
#4395 = CARTESIAN_POINT ( 'NONE',  ( 129.9999999999999432, -34.99999999999999289, -125.0000000000000000 ) ) ;
#4396 = LINE ( 'NONE', #17366, #10271 ) ;
#4397 = PLANE ( 'NONE',  #5224 ) ;
#4398 = CARTESIAN_POINT ( 'NONE',  ( 10.00000000000000000, 0.000000000000000000, 0.000000000000000000 ) ) ;
#4399 = ORIENTED_EDGE ( 'NONE', *, *, #11819, .T. ) ;
#4400 = FACE_OUTER_BOUND ( 'NONE', #15739, .T. ) ;
#4401 = EDGE_LOOP ( 'NONE', ( #2172, #17997, #14505, #6791 ) ) ;
#4402 = DIRECTION ( 'NONE',  ( 0.000000000000000000, 0.000000000000000000, 1.000000000000000000 ) ) ;
#4403 = CYLINDRICAL_SURFACE ( 'NONE', #10590, 2.100000000000000089 ) ;
#4404 = EDGE_LOOP ( 'NONE', ( #5392, #18272 ) ) ;
#4405 = EDGE_CURVE ( 'NONE', #5391, #4113, #4702, .T. ) ;
#4406 = ORIENTED_EDGE ( 'NONE', *, *, #8194, .T. ) ;
#4407 = AXIS2_PLACEMENT_3D ( 'NONE', #3295, #4622, #16061 ) ;
#4408 = ORIENTED_EDGE ( 'NONE', *, *, #15757, .T. ) ;
#4409 = DIRECTION ( 'NONE',  ( -1.000000000000000000, 0.000000000000000000, 0.000000000000000000 ) ) ;
#4410 = CARTESIAN_POINT ( 'NONE',  ( 0.000000000000000000, -27.72801475327278453, -5.086963483077506787 ) ) ;
#4411 = LINE ( 'NONE', #8519, #15149 ) ;
#4412 = ADVANCED_FACE ( 'NONE', ( #13572 ), #7653, .F. ) ;
#4413 = DIRECTION ( 'NONE',  ( 1.000000000000000000, 0.000000000000000000, 0.000000000000000000 ) ) ;
#4414 = DIRECTION ( 'NONE',  ( 0.1586811557617541224, -1.606889522083433522E-16, 0.9873298794253690946 ) ) ;
#4415 = CARTESIAN_POINT ( 'NONE',  ( 10.00000000000000000, -24.33982105418865061, -50.71018745830470920 ) ) ;
#4416 = CARTESIAN_POINT ( 'NONE',  ( -79.64793068852898728, -30.00000000000000000, -31.86039329588756530 ) ) ;
#4417 = EDGE_LOOP ( 'NONE', ( #16850, #18187, #10692, #6710, #7547 ) ) ;
#4418 = EDGE_CURVE ( 'NONE', #17588, #432, #3835, .T. ) ;
#4419 = AXIS2_PLACEMENT_3D ( 'NONE', #6994, #12517, #15656 ) ;
#4420 =( NAMED_UNIT ( * ) PLANE_ANGLE_UNIT ( ) SI_UNIT ( $, .RADIAN. ) );
#4421 = CARTESIAN_POINT ( 'NONE',  ( 0.000000000000000000, -34.99999999999999289, 0.000000000000000000 ) ) ;
#4422 = CARTESIAN_POINT ( 'NONE',  ( -10.00000000000000000, -26.45033635316118747, 39.05576474687271116 ) ) ;
#4423 = ORIENTED_EDGE ( 'NONE', *, *, #10677, .T. ) ;
#4424 = VECTOR ( 'NONE', #9470, 1000.000000000000000 ) ;
#4425 = ORIENTED_EDGE ( 'NONE', *, *, #4303, .T. ) ;
#4426 = CARTESIAN_POINT ( 'NONE',  ( 10.00000000000000000, -55.51919907100660367, 9.823366686500467182 ) ) ;
#4427 = SURFACE_STYLE_USAGE ( .BOTH. , #17312 ) ;
#4428 = ORIENTED_EDGE ( 'NONE', *, *, #10607, .T. ) ;
#4429 = CIRCLE ( 'NONE', #8990, 24.00000000002399858 ) ;
#4430 = VERTEX_POINT ( 'NONE', #4231 ) ;
#4431 = CARTESIAN_POINT ( 'NONE',  ( 10.00000000000000000, -47.29147401531925965, -41.62350880771970196 ) ) ;
#4432 = EDGE_CURVE ( 'NONE', #8867, #7847, #3189, .T. ) ;
#4433 = DIRECTION ( 'NONE',  ( -1.000000000000000000, 0.000000000000000000, 0.000000000000000000 ) ) ;
#4434 = VECTOR ( 'NONE', #2609, 1000.000000000000114 ) ;
#4435 = LINE ( 'NONE', #8907, #14208 ) ;
#4436 = VERTEX_POINT ( 'NONE', #4899 ) ;
#4437 = CARTESIAN_POINT ( 'NONE',  ( -2.250000000000000000, -27.60846790388774608, -2.000000000000000000 ) ) ;
#4438 = ORIENTED_EDGE ( 'NONE', *, *, #17189, .F. ) ;
#4439 = DIRECTION ( 'NONE',  ( -0.000000000000000000, 1.000000000000000000, -0.000000000000000000 ) ) ;
#4440 = ORIENTED_EDGE ( 'NONE', *, *, #15992, .T. ) ;
#4441 = ORIENTED_EDGE ( 'NONE', *, *, #18443, .F. ) ;
#4442 = DIRECTION ( 'NONE',  ( 0.000000000000000000, 0.000000000000000000, 1.000000000000000000 ) ) ;
#4443 = CARTESIAN_POINT ( 'NONE',  ( -4.000000000000000000, 2.309401076758498483, -5.000000000000000000 ) ) ;
#4444 = VECTOR ( 'NONE', #8898, 1000.000000000000000 ) ;
#4445 = VERTEX_POINT ( 'NONE', #1657 ) ;
#4446 = ORIENTED_EDGE ( 'NONE', *, *, #17557, .T. ) ;
#4447 = CIRCLE ( 'NONE', #15101, 12.00000000001200462 ) ;
#4448 = DIRECTION ( 'NONE',  ( 0.000000000000000000, 0.000000000000000000, 1.000000000000000000 ) ) ;
#4449 = SHAPE_REPRESENTATION_RELATIONSHIP ( 'NONE' , 'NONE' ,  #11521, #574 ) ;
#4450 = CIRCLE ( 'NONE', #2945, 24.00000000002399503 ) ;
#4451 = EDGE_LOOP ( 'NONE', ( #13837, #7550, #10937, #14970 ) ) ;
#4452 = DIRECTION ( 'NONE',  ( 0.5000000000000022204, 0.8660254037844374864, -0.000000000000000000 ) ) ;
#4453 = AXIS2_PLACEMENT_3D ( 'NONE', #18592, #8583, #4115 ) ;
#4454 = AXIS2_PLACEMENT_3D ( 'NONE', #4720, #10532, #439 ) ;
#4455 = EDGE_CURVE ( 'NONE', #5480, #12173, #7489, .T. ) ;
#4456 = EDGE_CURVE ( 'NONE', #5675, #10144, #11856, .T. ) ;
#4457 = CARTESIAN_POINT ( 'NONE',  ( 0.000000000000000000, 13.24999999999999467, 0.000000000000000000 ) ) ;
#4458 = EDGE_CURVE ( 'NONE', #9593, #14358, #12660, .T. ) ;
#4459 = AXIS2_PLACEMENT_3D ( 'NONE', #6944, #9796, #5312 ) ;
#4460 = ORIENTED_EDGE ( 'NONE', *, *, #7857, .T. ) ;
#4461 = CIRCLE ( 'NONE', #15119, 56.24900000005625600 ) ;
#4462 = EDGE_CURVE ( 'NONE', #17285, #14160, #6227, .T. ) ;
#4463 = VERTEX_POINT ( 'NONE', #12032 ) ;
#4464 = FACE_OUTER_BOUND ( 'NONE', #5126, .T. ) ;
#4465 = AXIS2_PLACEMENT_3D ( 'NONE', #5371, #9941, #15755 ) ;
#4466 = CARTESIAN_POINT ( 'NONE',  ( 0.000000000000000000, 29.03656532225586062, -15.68049343255964878 ) ) ;
#4467 = CARTESIAN_POINT ( 'NONE',  ( 5.000000000000000000, -40.19788616105644508, 48.50907078259368888 ) ) ;
#4468 = EDGE_LOOP ( 'NONE', ( #17730, #15846 ) ) ;
#4469 = CARTESIAN_POINT ( 'NONE',  ( -117.1020693116506379, -38.00000000000000000, -17.04080595179801705 ) ) ;
#4470 = EDGE_CURVE ( 'NONE', #6348, #10144, #13576, .T. ) ;
#4471 = CARTESIAN_POINT ( 'NONE',  ( -4.000000000000000000, -2.309401076758512694, -3.433295621305382461 ) ) ;
#4472 = CARTESIAN_POINT ( 'NONE',  ( 5.000000000000000000, -53.22058882792220658, 33.71303790549256263 ) ) ;
#4473 = CARTESIAN_POINT ( 'NONE',  ( 0.000000000000000000, 46.27827401617403780, 31.97297851452440653 ) ) ;
#4474 = ORIENTED_EDGE ( 'NONE', *, *, #14602, .F. ) ;
#4475 = DIRECTION ( 'NONE',  ( -1.000000000000000000, -0.000000000000000000, 0.000000000000000000 ) ) ;
#4476 =( LENGTH_UNIT ( ) NAMED_UNIT ( * ) SI_UNIT ( .MILLI., .METRE. ) );
#4477 = ADVANCED_FACE ( 'NONE', ( #10613 ), #16519, .T. ) ;
#4478 = ORIENTED_EDGE ( 'NONE', *, *, #67, .T. ) ;
#4479 = CARTESIAN_POINT ( 'NONE',  ( -36.40576474687271258, 10.00000000000000000, -26.45033635316118747 ) ) ;
#4480 = DIRECTION ( 'NONE',  ( -1.000000000000000000, -0.000000000000000000, -0.000000000000000000 ) ) ;
#4481 = VECTOR ( 'NONE', #16653, 1000.000000000000000 ) ;
#4482 = AXIS2_PLACEMENT_3D ( 'NONE', #17344, #13229, #14463 ) ;
#4483 = VECTOR ( 'NONE', #9098, 1000.000000000000000 ) ;
#4484 = CIRCLE ( 'NONE', #3582, 2.649999999999995914 ) ;
#4485 = EDGE_CURVE ( 'NONE', #5915, #18103, #6878, .T. ) ;
#4486 = VERTEX_POINT ( 'NONE', #6045 ) ;
#4487 = DIRECTION ( 'NONE',  ( -1.000000000000000000, -0.000000000000000000, -0.000000000000000000 ) ) ;
#4488 = FACE_OUTER_BOUND ( 'NONE', #14426, .T. ) ;
#4489 = AXIS2_PLACEMENT_3D ( 'NONE', #2259, #8072, #2544 ) ;
#4490 = VERTEX_POINT ( 'NONE', #11764 ) ;
#4491 =( LENGTH_UNIT ( ) NAMED_UNIT ( * ) SI_UNIT ( .MILLI., .METRE. ) );
#4492 = EDGE_CURVE ( 'NONE', #752, #6265, #16148, .T. ) ;
#4493 = CARTESIAN_POINT ( 'NONE',  ( 0.000000000000000000, -30.00000000000000000, 0.000000000000000000 ) ) ;
#4494 = AXIS2_PLACEMENT_3D ( 'NONE', #10696, #1939, #12223 ) ;
#4495 = DIRECTION ( 'NONE',  ( 0.000000000000000000, 0.000000000000000000, 1.000000000000000000 ) ) ;
#4496 = CARTESIAN_POINT ( 'NONE',  ( -0.1481481481481481122, -4.797713218419819903, -1.000000000000000000 ) ) ;
#4497 = AXIS2_PLACEMENT_3D ( 'NONE', #11576, #2805, #16137 ) ;
#4498 = CARTESIAN_POINT ( 'NONE',  ( 10.00000000000000000, 15.68049343256038064, -29.03656532225546627 ) ) ;
#4499 = VERTEX_POINT ( 'NONE', #14709 ) ;
#4500 = VECTOR ( 'NONE', #16574, 1000.000000000000000 ) ;
#4501 = LINE ( 'NONE', #213, #17922 ) ;
#4502 = VERTEX_POINT ( 'NONE', #16238 ) ;
#4503 = PRODUCT_DEFINITION_SHAPE ( 'NONE', 'NONE',  #18812 ) ;
#4504 =( NAMED_UNIT ( * ) PLANE_ANGLE_UNIT ( ) SI_UNIT ( $, .RADIAN. ) );
#4505 = DIRECTION ( 'NONE',  ( 0.000000000000000000, 0.9510565162951523099, 0.3090169943749515591 ) ) ;
#4506 = ORIENTED_EDGE ( 'NONE', *, *, #9915, .T. ) ;
#4507 = SHAPE_DEFINITION_REPRESENTATION ( #5861, #11521 ) ;
#4508 = ORIENTED_EDGE ( 'NONE', *, *, #1856, .F. ) ;
#4509 = VECTOR ( 'NONE', #10191, 1000.000000000000000 ) ;
#4510 = AXIS2_PLACEMENT_3D ( 'NONE', #14298, #10096, #13230 ) ;
#4511 = CARTESIAN_POINT ( 'NONE',  ( -90.00000000009001155, -49.14213562373095812, -1.301042606982603940E-15 ) ) ;
#4512 = FACE_OUTER_BOUND ( 'NONE', #14918, .T. ) ;
#4513 = DIRECTION ( 'NONE',  ( -1.000000000000000000, -0.000000000000000000, 0.000000000000000000 ) ) ;
#4514 = ADVANCED_FACE ( 'NONE', ( #17669 ), #336, .T. ) ;
#4515 = DIRECTION ( 'NONE',  ( 0.000000000000000000, 0.000000000000000000, 1.000000000000000000 ) ) ;
#4516 = CARTESIAN_POINT ( 'NONE',  ( -0.5000000000000000000, -6.429618962271402616, -1.000000000000000000 ) ) ;
#4517 = AXIS2_PLACEMENT_3D ( 'NONE', #2881, #10122, #2595 ) ;
#4518 = DIRECTION ( 'NONE',  ( 1.000000000000000000, 0.000000000000000000, 0.000000000000000000 ) ) ;
#4519 = CYLINDRICAL_SURFACE ( 'NONE', #264, 26.24900000002624978 ) ;
#4520 = ORIENTED_EDGE ( 'NONE', *, *, #15588, .T. ) ;
#4521 = AXIS2_PLACEMENT_3D ( 'NONE', #8761, #7333, #3057 ) ;
#4522 = DIRECTION ( 'NONE',  ( 1.000000000000000000, 0.000000000000000000, 0.000000000000000000 ) ) ;
#4523 = DIRECTION ( 'NONE',  ( 0.000000000000000000, -1.000000000000000000, 0.000000000000000000 ) ) ;
#4524 = DIRECTION ( 'NONE',  ( -1.000000000000000000, -0.000000000000000000, 0.000000000000000000 ) ) ;
#4525 = ORIENTED_EDGE ( 'NONE', *, *, #7230, .F. ) ;
#4526 = EDGE_LOOP ( 'NONE', ( #1388, #8069, #17436, #13082 ) ) ;
#4527 = VECTOR ( 'NONE', #5420, 1000.000000000000000 ) ;
#4528 = DIRECTION ( 'NONE',  ( -1.000000000000000000, 0.000000000000000000, 0.000000000000000000 ) ) ;
#4529 = CARTESIAN_POINT ( 'NONE',  ( 2.500000000000000000, 2.357898499370431722, -2.818925648462311528E-15 ) ) ;
#4530 = ORIENTED_EDGE ( 'NONE', *, *, #17601, .F. ) ;
#4531 = ADVANCED_FACE ( 'NONE', ( #6799 ), #3574, .T. ) ;
#4532 = AXIS2_PLACEMENT_3D ( 'NONE', #778, #8208, #14010 ) ;
#4533 = ADVANCED_FACE ( 'NONE', ( #11174 ), #13754, .T. ) ;
#4534 = DIRECTION ( 'NONE',  ( -1.000000000000000000, 0.000000000000000000, -0.000000000000000000 ) ) ;
#4535 = CYLINDRICAL_SURFACE ( 'NONE', #8962, 0.7500000000000000000 ) ;
#4536 = CARTESIAN_POINT ( 'NONE',  ( 0.000000000000000000, 26.20671763660628528, -1.489278925039611901 ) ) ;
#4537 = ORIENTED_EDGE ( 'NONE', *, *, #8008, .T. ) ;
#4538 = DIRECTION ( 'NONE',  ( -1.000000000000000000, -0.000000000000000000, -0.000000000000000000 ) ) ;
#4539 = ORIENTED_EDGE ( 'NONE', *, *, #8599, .T. ) ;
#4540 = FACE_OUTER_BOUND ( 'NONE', #4081, .T. ) ;
#4541 = ORIENTED_EDGE ( 'NONE', *, *, #1389, .T. ) ;
#4542 = CYLINDRICAL_SURFACE ( 'NONE', #14192, 20.00000000000000000 ) ;
#4543 = CARTESIAN_POINT ( 'NONE',  ( 10.00000000000000000, 40.70683587897958944, 38.81885513160003143 ) ) ;
#4544 = VECTOR ( 'NONE', #5333, 1000.000000000000000 ) ;
#4545 = ORIENTED_EDGE ( 'NONE', *, *, #10984, .F. ) ;
#4546 = ORIENTED_EDGE ( 'NONE', *, *, #11100, .T. ) ;
#4547 = CARTESIAN_POINT ( 'NONE',  ( 10.00000000000000000, 55.74967257055883607, 7.478235706489176238 ) ) ;
#4548 = CIRCLE ( 'NONE', #17627, 12.00000000001200640 ) ;
#4549 = EDGE_LOOP ( 'NONE', ( #992, #4614, #495, #17288 ) ) ;
#4550 = DIRECTION ( 'NONE',  ( -1.000000000000000000, -0.000000000000000000, 0.000000000000000000 ) ) ;
#4551 = FACE_OUTER_BOUND ( 'NONE', #17127, .T. ) ;
#4552 = AXIS2_PLACEMENT_3D ( 'NONE', #9959, #11761, #10235 ) ;
#4553 = ORIENTED_EDGE ( 'NONE', *, *, #13299, .F. ) ;
#4554 = CIRCLE ( 'NONE', #3043, 2.649999999999999467 ) ;
#4555 = EDGE_LOOP ( 'NONE', ( #11172, #10972, #14571, #7323 ) ) ;
#4556 = CARTESIAN_POINT ( 'NONE',  ( -11.25000000000000355, 0.000000000000000000, 0.000000000000000000 ) ) ;
#4557 = DIRECTION ( 'NONE',  ( -0.000000000000000000, -1.000000000000000000, -0.000000000000000000 ) ) ;
#4558 = DIRECTION ( 'NONE',  ( 1.000000000000000000, 0.000000000000000000, 0.000000000000000000 ) ) ;
#4559 = ORIENTED_EDGE ( 'NONE', *, *, #12967, .T. ) ;
#4560 = CARTESIAN_POINT ( 'NONE',  ( -4.000000000000000000, -0.8232339106130515116, -3.430630286862743183 ) ) ;
#4561 = DIRECTION ( 'NONE',  ( -1.000000000000000000, 0.000000000000000000, -0.000000000000000000 ) ) ;
#4562 = CARTESIAN_POINT ( 'NONE',  ( 5.000000000000000000, 32.11449294037271329, -54.20017844242479299 ) ) ;
#4563 = FACE_BOUND ( 'NONE', #1833, .T. ) ;
#4564 = VERTEX_POINT ( 'NONE', #18406 ) ;
#4565 = CARTESIAN_POINT ( 'NONE',  ( 0.000000000000000000, 32.70783759231086663, 4.381479206523104963 ) ) ;
#4566 = EDGE_CURVE ( 'NONE', #9120, #8129, #15709, .T. ) ;
#4567 = DIRECTION ( 'NONE',  ( -1.000000000000000000, 0.000000000000000000, -0.000000000000000000 ) ) ;
#4568 = EDGE_CURVE ( 'NONE', #3665, #4445, #5049, .T. ) ;
#4569 = ORIENTED_EDGE ( 'NONE', *, *, #14938, .T. ) ;
#4570 = LINE ( 'NONE', #5994, #3321 ) ;
#4571 = DIRECTION ( 'NONE',  ( -1.000000000000000000, 0.000000000000000000, -0.000000000000000000 ) ) ;
#4572 = AXIS2_PLACEMENT_3D ( 'NONE', #16701, #3653, #9449 ) ;
#4573 = CIRCLE ( 'NONE', #14624, 2.041999999999999815 ) ;
#4574 = EDGE_CURVE ( 'NONE', #13860, #11877, #18493, .T. ) ;
#4575 = EDGE_CURVE ( 'NONE', #5775, #18341, #9926, .T. ) ;
#4576 = ORIENTED_EDGE ( 'NONE', *, *, #8347, .F. ) ;
#4577 = DIRECTION ( 'NONE',  ( -1.000000000000000000, 0.000000000000000000, 0.000000000000000000 ) ) ;
#4578 = CARTESIAN_POINT ( 'NONE',  ( 0.000000000000000000, 3.000000000000000000, 0.000000000000000000 ) ) ;
#4579 = EDGE_CURVE ( 'NONE', #4113, #18014, #15100, .T. ) ;
#4580 = ORIENTED_EDGE ( 'NONE', *, *, #13871, .F. ) ;
#4581 =( NAMED_UNIT ( * ) PLANE_ANGLE_UNIT ( ) SI_UNIT ( $, .RADIAN. ) );
#4582 = DIRECTION ( 'NONE',  ( 0.000000000000000000, 0.000000000000000000, 1.000000000000000000 ) ) ;
#4583 = VECTOR ( 'NONE', #3350, 1000.000000000000114 ) ;
#4584 = CARTESIAN_POINT ( 'NONE',  ( -90.00000000009001155, -38.00000000000000000, 40.00000000000000000 ) ) ;
#4585 = FACE_OUTER_BOUND ( 'NONE', #12863, .T. ) ;
#4586 = CARTESIAN_POINT ( 'NONE',  ( -26.29305231718584324, -26.50000000000000000, 21.75302069950530637 ) ) ;
#4587 = ORIENTED_EDGE ( 'NONE', *, *, #9763, .T. ) ;
#4588 = DIRECTION ( 'NONE',  ( 1.000000000000000000, 0.000000000000000000, 0.000000000000000000 ) ) ;
#4589 = ORIENTED_EDGE ( 'NONE', *, *, #8242, .F. ) ;
#4590 = EDGE_CURVE ( 'NONE', #16471, #3732, #489, .T. ) ;
#4591 = EDGE_CURVE ( 'NONE', #6386, #6721, #12602, .T. ) ;
#4592 = DIRECTION ( 'NONE',  ( 0.000000000000000000, 1.000000000000000000, 0.000000000000000000 ) ) ;
#4593 = ORIENTED_EDGE ( 'NONE', *, *, #3280, .F. ) ;
#4594 = CONTEXT_DEPENDENT_SHAPE_REPRESENTATION ( #10361, #11646 ) ;
#4595 = ADVANCED_FACE ( 'NONE', ( #13947 ), #13670, .T. ) ;
#4596 = ORIENTED_EDGE ( 'NONE', *, *, #8367, .F. ) ;
#4597 = ADVANCED_FACE ( 'NONE', ( #7848 ), #616, .F. ) ;
#4598 = ORIENTED_EDGE ( 'NONE', *, *, #18297, .F. ) ;
#4599 = VERTEX_POINT ( 'NONE', #2319 ) ;
#4600 = DIRECTION ( 'NONE',  ( 0.000000000000000000, -1.000000000000000000, 0.000000000000000000 ) ) ;
#4601 = LINE ( 'NONE', #5763, #13394 ) ;
#4602 = DIRECTION ( 'NONE',  ( 0.000000000000000000, 0.000000000000000000, 1.000000000000000000 ) ) ;
#4603 = DIRECTION ( 'NONE',  ( -0.000000000000000000, 1.000000000000000000, -0.000000000000000000 ) ) ;
#4604 = DIRECTION ( 'NONE',  ( 0.000000000000000000, 0.000000000000000000, 1.000000000000000000 ) ) ;
#4605 = DIRECTION ( 'NONE',  ( -0.000000000000000000, 1.000000000000000000, -0.000000000000000000 ) ) ;
#4606 = DIRECTION ( 'NONE',  ( 0.000000000000000000, -1.000000000000000000, 0.000000000000000000 ) ) ;
#4607 = CARTESIAN_POINT ( 'NONE',  ( 0.000000000000000000, 0.000000000000000000, -4.000000000000000000 ) ) ;
#4608 = ORIENTED_EDGE ( 'NONE', *, *, #1240, .T. ) ;
#4609 = CIRCLE ( 'NONE', #3671, 63.00000000006298961 ) ;
#4610 = DIRECTION ( 'NONE',  ( -0.000000000000000000, 1.000000000000000000, 0.000000000000000000 ) ) ;
#4611 = DIRECTION ( 'NONE',  ( -1.000000000000000000, 0.000000000000000000, -0.000000000000000000 ) ) ;
#4612 = FACE_OUTER_BOUND ( 'NONE', #11902, .T. ) ;
#4613 = ORIENTED_EDGE ( 'NONE', *, *, #12615, .T. ) ;
#4614 = ORIENTED_EDGE ( 'NONE', *, *, #7486, .F. ) ;
#4615 = CARTESIAN_POINT ( 'NONE',  ( -3.680118525130244400, 2.494084732383327285, -0.3507732604232449702 ) ) ;
#4616 = VECTOR ( 'NONE', #13165, 1000.000000000000000 ) ;
#4617 = CARTESIAN_POINT ( 'NONE',  ( 10.00000000000000000, 0.000000000000000000, 0.000000000000000000 ) ) ;
#4618 = ORIENTED_EDGE ( 'NONE', *, *, #13445, .T. ) ;
#4619 = AXIS2_PLACEMENT_3D ( 'NONE', #9800, #2558, #1146 ) ;
#4620 = ADVANCED_FACE ( 'NONE', ( #15272 ), #14041, .T. ) ;
#4621 = DIRECTION ( 'NONE',  ( 0.1305261922200524616, -0.9914448613738103822, 0.000000000000000000 ) ) ;
#4622 = DIRECTION ( 'NONE',  ( -1.000000000000000000, -0.000000000000000000, 0.000000000000000000 ) ) ;
#4623 = DIRECTION ( 'NONE',  ( -1.000000000000000000, -0.000000000000000000, -0.000000000000000000 ) ) ;
#4624 = ORIENTED_EDGE ( 'NONE', *, *, #12143, .F. ) ;
#4625 = DIRECTION ( 'NONE',  ( 0.000000000000000000, 0.000000000000000000, 1.000000000000000000 ) ) ;
#4626 = AXIS2_PLACEMENT_3D ( 'NONE', #10086, #14735, #10172 ) ;
#4627 = ORIENTED_EDGE ( 'NONE', *, *, #2549, .T. ) ;
#4628 = CYLINDRICAL_SURFACE ( 'NONE', #2378, 12.00000000001200462 ) ;
#4629 = ORIENTED_EDGE ( 'NONE', *, *, #9515, .F. ) ;
#4630 = APPLICATION_CONTEXT ( 'automotive_design' ) ;
#4631 = EDGE_CURVE ( 'NONE', #5290, #5739, #12349, .T. ) ;
#4632 = DIRECTION ( 'NONE',  ( -1.000000000000000000, -0.000000000000000000, 0.000000000000000000 ) ) ;
#4633 = CARTESIAN_POINT ( 'NONE',  ( 2.805705207896068476, -3.226868319750173075, -3.503898532754370354 ) ) ;
#4634 = ORIENTED_EDGE ( 'NONE', *, *, #6742, .T. ) ;
#4635 = ORIENTED_EDGE ( 'NONE', *, *, #15519, .F. ) ;
#4636 = CARTESIAN_POINT ( 'NONE',  ( 0.000000000000000000, 53.92768374110892893, -16.45250512421876010 ) ) ;
#4637 = EDGE_CURVE ( 'NONE', #8129, #11016, #7191, .T. ) ;
#4638 = PRESENTATION_STYLE_ASSIGNMENT (( #15973 ) ) ;
#4639 = ORIENTED_EDGE ( 'NONE', *, *, #15062, .T. ) ;
#4640 = DIRECTION ( 'NONE',  ( 0.000000000000000000, 0.000000000000000000, 1.000000000000000000 ) ) ;
#4641 = AXIS2_PLACEMENT_3D ( 'NONE', #5514, #17137, #12846 ) ;
#4642 = VECTOR ( 'NONE', #16317, 1000.000000000000000 ) ;
#4643 = DIRECTION ( 'NONE',  ( 0.000000000000000000, 0.000000000000000000, 1.000000000000000000 ) ) ;
#4644 = VERTEX_POINT ( 'NONE', #18232 ) ;
#4645 = ORIENTED_EDGE ( 'NONE', *, *, #13090, .F. ) ;
#4646 = DIRECTION ( 'NONE',  ( 0.000000000000000000, 0.000000000000000000, -1.000000000000000000 ) ) ;
#4647 = FACE_OUTER_BOUND ( 'NONE', #16602, .T. ) ;
#4648 = CARTESIAN_POINT ( 'NONE',  ( 0.000000000000000000, 7.478235706489786416, -55.74967257055873660 ) ) ;
#4649 = EDGE_CURVE ( 'NONE', #9984, #16064, #4164, .T. ) ;
#4650 = EDGE_LOOP ( 'NONE', ( #17700, #17577, #9418, #7806 ) ) ;
#4651 = CARTESIAN_POINT ( 'NONE',  ( 10.00000000000000000, 0.000000000000000000, 0.000000000000000000 ) ) ;
#4652 = CIRCLE ( 'NONE', #8306, 24.00000000002400213 ) ;
#4653 = DIRECTION ( 'NONE',  ( 0.000000000000000000, 0.000000000000000000, -1.000000000000000000 ) ) ;
#4654 = CARTESIAN_POINT ( 'NONE',  ( 10.00000000000000000, -39.14194549634393638, 40.58063702438330722 ) ) ;
#4655 = LINE ( 'NONE', #11623, #18127 ) ;
#4656 = ORIENTED_EDGE ( 'NONE', *, *, #10520, .T. ) ;
#4657 = CIRCLE ( 'NONE', #7088, 2.649999999999999467 ) ;
#4658 = DIRECTION ( 'NONE',  ( 0.000000000000000000, 0.000000000000000000, 1.000000000000000000 ) ) ;
#4659 = CYLINDRICAL_SURFACE ( 'NONE', #5374, 12.00000000001200462 ) ;
#4660 = ADVANCED_FACE ( 'NONE', ( #18607 ), #9846, .T. ) ;
#4661 = VERTEX_POINT ( 'NONE', #15655 ) ;
#4662 = CYLINDRICAL_SURFACE ( 'NONE', #14552, 2.649999999999999467 ) ;
#4663 = DIRECTION ( 'NONE',  ( 0.000000000000000000, 0.000000000000000000, 1.000000000000000000 ) ) ;
#4664 = CIRCLE ( 'NONE', #18360, 56.24900000005626310 ) ;
#4665 = EDGE_CURVE ( 'NONE', #14075, #7866, #17832, .T. ) ;
#4666 = VERTEX_POINT ( 'NONE', #9939 ) ;
#4667 = CARTESIAN_POINT ( 'NONE',  ( 0.000000000000000000, 0.000000000000000000, -2.000000000000000000 ) ) ;
#4668 = EDGE_CURVE ( 'NONE', #5686, #14039, #16614, .T. ) ;
#4669 = CARTESIAN_POINT ( 'NONE',  ( 10.00000000000000000, 0.000000000000000000, 0.000000000000000000 ) ) ;
#4670 = ORIENTED_EDGE ( 'NONE', *, *, #6303, .T. ) ;
#4671 = CARTESIAN_POINT ( 'NONE',  ( 0.000000000000000000, 25.38428207620331634, -6.681932690256706664 ) ) ;
#4672 = CARTESIAN_POINT ( 'NONE',  ( 0.000000000000000000, 46.27827401617449965, -31.97297851452373507 ) ) ;
#4673 = PRODUCT_DEFINITION ( 'UNKNOWN', '', #8673, #14538 ) ;
#4674 = CARTESIAN_POINT ( 'NONE',  ( 0.000000000000000000, 16.10733642026559309, -53.89344778774794520 ) ) ;
#4675 = LINE ( 'NONE', #15056, #11302 ) ;
#4676 = ORIENTED_EDGE ( 'NONE', *, *, #8560, .T. ) ;
#4677 = CARTESIAN_POINT ( 'NONE',  ( 0.000000000000000000, 0.000000000000000000, -25.03750572909317285 ) ) ;
#4678 = ORIENTED_EDGE ( 'NONE', *, *, #10356, .F. ) ;
#4679 = DIRECTION ( 'NONE',  ( 1.000000000000000000, 0.000000000000000000, 0.000000000000000000 ) ) ;
#4680 = EDGE_LOOP ( 'NONE', ( #12179, #18446, #11092 ) ) ;
#4681 = ORIENTED_EDGE ( 'NONE', *, *, #9594, .F. ) ;
#4682 = ORIENTED_EDGE ( 'NONE', *, *, #1308, .T. ) ;
#4683 = ADVANCED_FACE ( 'NONE', ( #12804 ), #2511, .T. ) ;
#4684 = ORIENTED_EDGE ( 'NONE', *, *, #10641, .F. ) ;
#4685 = PRESENTATION_LAYER_ASSIGNMENT (  '', '', ( #1957 ) ) ;
#4686 = FACE_OUTER_BOUND ( 'NONE', #2018, .T. ) ;
#4687 = EDGE_CURVE ( 'NONE', #8217, #10632, #814, .T. ) ;
#4688 = EDGE_CURVE ( 'NONE', #3720, #17733, #11276, .T. ) ;
#4689 = CARTESIAN_POINT ( 'NONE',  ( 10.00000000000000000, -26.20671763660627462, -1.489278925039791535 ) ) ;
#4690 = DIRECTION ( 'NONE',  ( 0.000000000000000000, 0.000000000000000000, 1.000000000000000000 ) ) ;
#4691 = CARTESIAN_POINT ( 'NONE',  ( 10.00000000000000000, -26.45033635316118747, 33.75576474687270689 ) ) ;
#4692 = ADVANCED_FACE ( 'NONE', ( #2601 ), #11454, .T. ) ;
#4693 = CARTESIAN_POINT ( 'NONE',  ( -3.500000000000000888, -27.60846790388774608, -2.000000000000000000 ) ) ;
#4694 = LINE ( 'NONE', #11934, #14995 ) ;
#4695 = DIRECTION ( 'NONE',  ( 0.000000000000000000, 0.000000000000000000, 1.000000000000000000 ) ) ;
#4696 = FACE_OUTER_BOUND ( 'NONE', #12160, .T. ) ;
#4697 = ORIENTED_EDGE ( 'NONE', *, *, #16389, .F. ) ;
#4698 = CARTESIAN_POINT ( 'NONE',  ( 4.211140560182196957, 2.431303136016536470, -3.745885042887433514 ) ) ;
#4699 = DIRECTION ( 'NONE',  ( -1.000000000000000000, 0.000000000000000000, 0.000000000000000000 ) ) ;
#4700 = ORIENTED_EDGE ( 'NONE', *, *, #5385, .T. ) ;
#4701 = ORIENTED_EDGE ( 'NONE', *, *, #15404, .T. ) ;
#4702 = LINE ( 'NONE', #1851, #15405 ) ;
#4703 = CARTESIAN_POINT ( 'NONE',  ( 0.000000000000000000, 0.000000000000000000, 0.000000000000000000 ) ) ;
#4704 = EDGE_CURVE ( 'NONE', #16890, #11456, #12037, .T. ) ;
#4705 = AXIS2_PLACEMENT_3D ( 'NONE', #14910, #13671, #15096 ) ;
#4706 = CARTESIAN_POINT ( 'NONE',  ( 11.25000000000000000, 3.667817163446322894E-15, -29.90000000000000213 ) ) ;
#4707 = ORIENTED_EDGE ( 'NONE', *, *, #3241, .T. ) ;
#4708 = CIRCLE ( 'NONE', #151, 2.649999999999999467 ) ;
#4709 = EDGE_CURVE ( 'NONE', #445, #5103, #3555, .T. ) ;
#4710 = CARTESIAN_POINT ( 'NONE',  ( 0.000000000000000000, 62.72529079327815538, -5.876895005581757481 ) ) ;
#4711 = LINE ( 'NONE', #3297, #4483 ) ;
#4712 = ORIENTED_EDGE ( 'NONE', *, *, #16738, .T. ) ;
#4713 = CARTESIAN_POINT ( 'NONE',  ( 10.00000000000000000, 32.31183295104839459, -46.20417134726096009 ) ) ;
#4714 = ORIENTED_EDGE ( 'NONE', *, *, #13299, .T. ) ;
#4715 = AXIS2_PLACEMENT_3D ( 'NONE', #10150, #6053, #13488 ) ;
#4716 = EDGE_LOOP ( 'NONE', ( #13734, #4288, #16408 ) ) ;
#4717 = LINE ( 'NONE', #16533, #15668 ) ;
#4718 = EDGE_LOOP ( 'NONE', ( #3340, #2880, #7402, #8722 ) ) ;
#4719 = ADVANCED_FACE ( 'NONE', ( #12379 ), #4007, .T. ) ;
#4720 = CARTESIAN_POINT ( 'NONE',  ( -10.00000000000000000, 0.000000000000000000, 0.000000000000000000 ) ) ;
#4721 = CARTESIAN_POINT ( 'NONE',  ( 0.000000000000000000, -5.086963483077402870, 27.72801475327280585 ) ) ;
#4722 = VERTEX_POINT ( 'NONE', #10944 ) ;
#4723 = ORIENTED_EDGE ( 'NONE', *, *, #15191, .F. ) ;
#4724 = CARTESIAN_POINT ( 'NONE',  ( -26.29305231718568336, -26.50000000000000000, -19.10302069950552095 ) ) ;
#4725 =( NAMED_UNIT ( * ) PLANE_ANGLE_UNIT ( ) SI_UNIT ( $, .RADIAN. ) );
#4726 = EDGE_LOOP ( 'NONE', ( #3806, #16728, #16453, #2316 ) ) ;
#4727 = CARTESIAN_POINT ( 'NONE',  ( -117.1020693116508085, -30.00000000000000000, 19.69080595179778115 ) ) ;
#4728 = CIRCLE ( 'NONE', #15680, 2.649999999999992806 ) ;
#4729 = DIRECTION ( 'NONE',  ( 0.000000000000000000, -6.938893903900287191E-15, 1.000000000000000000 ) ) ;
#4730 = CIRCLE ( 'NONE', #6561, 56.24900000005627732 ) ;
#4731 = CIRCLE ( 'NONE', #10803, 12.00000000001200462 ) ;
#4732 = LINE ( 'NONE', #15220, #11719 ) ;
#4733 = ORIENTED_EDGE ( 'NONE', *, *, #13486, .T. ) ;
#4734 = AXIS2_PLACEMENT_3D ( 'NONE', #4724, #443, #6356 ) ;
#4735 = ORIENTED_EDGE ( 'NONE', *, *, #8304, .F. ) ;
#4736 = CARTESIAN_POINT ( 'NONE',  ( -117.1020693116508085, -30.00000000000000000, 19.69080595179778115 ) ) ;
#4737 = FACE_OUTER_BOUND ( 'NONE', #4401, .T. ) ;
#4739 = CIRCLE ( 'NONE', #9294, 63.00000000006298961 ) ;
#4738 = DIRECTION ( 'NONE',  ( 1.000000000000000000, 0.000000000000000000, 0.000000000000000000 ) ) ;
#4740 = ORIENTED_EDGE ( 'NONE', *, *, #11222, .F. ) ;
#4741 = CARTESIAN_POINT ( 'NONE',  ( -3.974357786152442180E-13, 4.796734841935204052, -3.721909803043259579 ) ) ;
#4742 = EDGE_CURVE ( 'NONE', #421, #6727, #6673, .T. ) ;
#4743 = VECTOR ( 'NONE', #15741, 1000.000000000000000 ) ;
#4744 = CARTESIAN_POINT ( 'NONE',  ( 10.00000000000000000, 0.000000000000000000, 0.000000000000000000 ) ) ;
#4745 = CYLINDRICAL_SURFACE ( 'NONE', #1306, 24.00000000002399503 ) ;
#4746 = CIRCLE ( 'NONE', #12973, 24.00000000002399858 ) ;
#4747 = CARTESIAN_POINT ( 'NONE',  ( 10.00000000000000000, -53.06836994729246726, 18.64666490672351529 ) ) ;
#4748 = ORIENTED_EDGE ( 'NONE', *, *, #4123, .F. ) ;
#4749 = DIRECTION ( 'NONE',  ( 0.000000000000000000, 1.000000000000000000, 0.000000000000000000 ) ) ;
#4750 = VECTOR ( 'NONE', #7871, 1000.000000000000000 ) ;
#4751 = AXIS2_PLACEMENT_3D ( 'NONE', #7811, #13635, #12196 ) ;
#4752 = FACE_OUTER_BOUND ( 'NONE', #13962, .T. ) ;
#4753 = EDGE_LOOP ( 'NONE', ( #15600, #9398, #8943, #15189 ) ) ;
#4754 = FACE_OUTER_BOUND ( 'NONE', #5207, .T. ) ;
#4755 = CARTESIAN_POINT ( 'NONE',  ( 0.000000000000000000, -17.25000000000000355, 0.000000000000000000 ) ) ;
#4756 = AXIS2_PLACEMENT_3D ( 'NONE', #4982, #16719, #712 ) ;
#4757 = EDGE_CURVE ( 'NONE', #8925, #3393, #15618, .T. ) ;
#4758 = CIRCLE ( 'NONE', #16943, 24.00000000002399858 ) ;
#4759 = AXIS2_PLACEMENT_3D ( 'NONE', #6871, #12690, #17168 ) ;
#4760 = VECTOR ( 'NONE', #1251, 1000.000000000000000 ) ;
#4761 = ORIENTED_EDGE ( 'NONE', *, *, #4839, .F. ) ;
#4762 = ADVANCED_FACE ( 'NONE', ( #672 ), #6759, .F. ) ;
#4763 = DIRECTION ( 'NONE',  ( 0.000000000000000000, 0.8090169943749445647, 0.5877852522924770229 ) ) ;
#4764 = EDGE_LOOP ( 'NONE', ( #17958, #10734 ) ) ;
#4765 = CARTESIAN_POINT ( 'NONE',  ( 50.00005079999999680, 0.000000000000000000, 0.000000000000000000 ) ) ;
#4766 = CARTESIAN_POINT ( 'NONE',  ( 0.000000000000000000, -55.83748330407401284, -7.813799127873885197 ) ) ;
#4767 = DIRECTION ( 'NONE',  ( -1.000000000000000000, -0.000000000000000000, 0.000000000000000000 ) ) ;
#4768 = CARTESIAN_POINT ( 'NONE',  ( 10.00000000000000000, -23.24033432160479862, 58.55669782892453412 ) ) ;
#4769 = AXIS2_PLACEMENT_3D ( 'NONE', #17245, #16087, #10275 ) ;
#4770 = DIRECTION ( 'NONE',  ( 1.000000000000000000, 0.000000000000000000, -0.000000000000000000 ) ) ;
#4771 = ORIENTED_EDGE ( 'NONE', *, *, #9423, .T. ) ;
#4772 = DIRECTION ( 'NONE',  ( 1.000000000000000000, 0.000000000000000000, 0.000000000000000000 ) ) ;
#4773 = VERTEX_POINT ( 'NONE', #1050 ) ;
#4774 = AXIS2_PLACEMENT_3D ( 'NONE', #12462, #9790, #854 ) ;
#4775 = SURFACE_STYLE_FILL_AREA ( #16406 ) ;
#4776 = CARTESIAN_POINT ( 'NONE',  ( 0.000000000000000000, -30.00000000000000000, 25.00000000000000000 ) ) ;
#4777 = ORIENTED_EDGE ( 'NONE', *, *, #13457, .F. ) ;
#4778 = VECTOR ( 'NONE', #844, 1000.000000000000000 ) ;
#4779 = AXIS2_PLACEMENT_3D ( 'NONE', #18068, #9407, #18167 ) ;
#4780 = ORIENTED_EDGE ( 'NONE', *, *, #8755, .T. ) ;
#4781 = VERTEX_POINT ( 'NONE', #13806 ) ;
#4782 = ORIENTED_EDGE ( 'NONE', *, *, #8424, .F. ) ;
#4783 = VECTOR ( 'NONE', #8234, 1000.000000000000000 ) ;
#4784 = DIRECTION ( 'NONE',  ( -1.000000000000000000, -0.000000000000000000, -0.000000000000000000 ) ) ;
#4785 =( LENGTH_UNIT ( ) NAMED_UNIT ( * ) SI_UNIT ( .MILLI., .METRE. ) );
#4786 = CIRCLE ( 'NONE', #2051, 12.00000000001200462 ) ;
#4787 = AXIS2_PLACEMENT_3D ( 'NONE', #3742, #903, #16792 ) ;
#4788 = CARTESIAN_POINT ( 'NONE',  ( 2.500000000000000000, 2.357898499370432166, -2.385244779468109755E-15 ) ) ;
#4789 = LINE ( 'NONE', #8799, #18571 ) ;
#4790 = DIRECTION ( 'NONE',  ( -1.000000000000000000, -0.000000000000000000, 0.000000000000000000 ) ) ;
#4791 = CARTESIAN_POINT ( 'NONE',  ( 11.14999999999999680, 0.000000000000000000, 0.000000000000000000 ) ) ;
#4792 = FACE_OUTER_BOUND ( 'NONE', #14817, .T. ) ;
#4793 = ORIENTED_EDGE ( 'NONE', *, *, #12813, .F. ) ;
#4794 = DIRECTION ( 'NONE',  ( 0.9873298794253685395, 0.000000000000000000, -0.1586811557617575918 ) ) ;
#4795 = ORIENTED_EDGE ( 'NONE', *, *, #6534, .F. ) ;
#4796 = DIRECTION ( 'NONE',  ( -0.000000000000000000, 1.000000000000000000, -0.000000000000000000 ) ) ;
#4797 = CARTESIAN_POINT ( 'NONE',  ( 10.04305231718579705, -26.50000000000000000, 30.90933677959249337 ) ) ;
#4798 = AXIS2_PLACEMENT_3D ( 'NONE', #7685, #13511, #455 ) ;
#4799 = ORIENTED_EDGE ( 'NONE', *, *, #14024, .F. ) ;
#4800 = VERTEX_POINT ( 'NONE', #16770 ) ;
#4801 = ADVANCED_FACE ( 'NONE', ( #3721 ), #9518, .T. ) ;
#4802 = EDGE_CURVE ( 'NONE', #12513, #8692, #9019, .T. ) ;
#4803 = DIRECTION ( 'NONE',  ( -1.000000000000000000, 0.000000000000000000, 0.000000000000000000 ) ) ;
#4804 = CARTESIAN_POINT ( 'NONE',  ( 0.000000000000000000, 0.000000000000000000, 0.000000000000000000 ) ) ;
#4805 = CIRCLE ( 'NONE', #15454, 24.00000000002400569 ) ;
#4807 = EDGE_CURVE ( 'NONE', #3732, #16471, #5062, .T. ) ;
#4806 = DIRECTION ( 'NONE',  ( 0.000000000000000000, 0.000000000000000000, -1.000000000000000000 ) ) ;
#4808 = ORIENTED_EDGE ( 'NONE', *, *, #2262, .T. ) ;
#4809 = VECTOR ( 'NONE', #4513, 1000.000000000000000 ) ;
#4810 = CIRCLE ( 'NONE', #13953, 4.349594641156948605 ) ;
#4811 = EDGE_CURVE ( 'NONE', #10374, #9128, #18772, .T. ) ;
#4812 = PRODUCT_DEFINITION_SHAPE ( 'NONE', 'NONE',  #18830 ) ;
#4813 = EDGE_CURVE ( 'NONE', #3285, #9916, #12067, .T. ) ;
#4814 = FACE_OUTER_BOUND ( 'NONE', #6738, .T. ) ;
#4815 = DIRECTION ( 'NONE',  ( -1.000000000000000000, 0.000000000000000000, 2.220446049250313081E-16 ) ) ;
#4816 = TOROIDAL_SURFACE ( 'NONE', #2686, 29.90000000000000213, 0.1000000000000011297 ) ;
#4817 = EDGE_CURVE ( 'NONE', #12768, #6721, #15427, .T. ) ;
#4818 = DIRECTION ( 'NONE',  ( 0.000000000000000000, -0.1564344650402382242, 0.9876883405951364381 ) ) ;
#4819 = VERTEX_POINT ( 'NONE', #9612 ) ;
#4820 = CARTESIAN_POINT ( 'NONE',  ( 3.349226789952652439, 2.685125164760731487, -0.2236248678334773199 ) ) ;
#4821 = AXIS2_PLACEMENT_3D ( 'NONE', #6753, #8084, #15043 ) ;
#4822 = EDGE_CURVE ( 'NONE', #3525, #7103, #8095, .T. ) ;
#4823 = AXIS2_PLACEMENT_3D ( 'NONE', #17657, #14894, #3174 ) ;
#4824 = ORIENTED_EDGE ( 'NONE', *, *, #1946, .F. ) ;
#4825 = AXIS2_PLACEMENT_3D ( 'NONE', #2858, #8657, #14465 ) ;
#4826 = DIRECTION ( 'NONE',  ( 0.000000000000000000, 0.1564344650402243464, 0.9876883405951388806 ) ) ;
#4827 = ORIENTED_EDGE ( 'NONE', *, *, #372, .T. ) ;
#4828 = CYLINDRICAL_SURFACE ( 'NONE', #9613, 0.7499999999999997780 ) ;
#4829 = CARTESIAN_POINT ( 'NONE',  ( -56.50000000009000445, -34.99999999999999289, 2.650000000000374278 ) ) ;
#4830 = ORIENTED_EDGE ( 'NONE', *, *, #14658, .F. ) ;
#4831 = VERTEX_POINT ( 'NONE', #11036 ) ;
#4832 = EDGE_CURVE ( 'NONE', #7722, #17686, #3252, .T. ) ;
#4833 = CYLINDRICAL_SURFACE ( 'NONE', #173, 24.00000000002399858 ) ;
#4834 = EDGE_CURVE ( 'NONE', #13484, #12910, #4172, .T. ) ;
#4835 = ORIENTED_EDGE ( 'NONE', *, *, #16007, .T. ) ;
#4836 = DIRECTION ( 'NONE',  ( 0.000000000000000000, 1.000000000000000000, 0.000000000000000000 ) ) ;
#4837 = AXIS2_PLACEMENT_3D ( 'NONE', #18708, #11579, #4331 ) ;
#4838 = AXIS2_PLACEMENT_3D ( 'NONE', #18488, #14472, #8490 ) ;
#4839 = EDGE_CURVE ( 'NONE', #4158, #6075, #1721, .T. ) ;
#4840 = CARTESIAN_POINT ( 'NONE',  ( -4.211140560182196957, 2.431303136016537803, -3.745885042887433514 ) ) ;
#4841 = ORIENTED_EDGE ( 'NONE', *, *, #6732, .T. ) ;
#4842 = ORIENTED_EDGE ( 'NONE', *, *, #5631, .F. ) ;
#4843 = DIRECTION ( 'NONE',  ( 0.000000000000000000, 0.000000000000000000, 1.000000000000000000 ) ) ;
#4844 = CARTESIAN_POINT ( 'NONE',  ( -26.29305231718584324, -30.00000000000000000, 16.45302069950530566 ) ) ;
#4845 = DIRECTION ( 'NONE',  ( 0.000000000000000000, -0.9510565162951565288, 0.3090169943749382919 ) ) ;
#4846 = ORIENTED_EDGE ( 'NONE', *, *, #14014, .T. ) ;
#4847 = CARTESIAN_POINT ( 'NONE',  ( 0.000000000000000000, 24.33982105418971642, -50.71018745830419050 ) ) ;
#4848 = CYLINDRICAL_SURFACE ( 'NONE', #16082, 63.00000000006298961 ) ;
#4849 = CARTESIAN_POINT ( 'NONE',  ( -90.00000000009001155, -13.00000000000001776, -1.691355389077386325E-15 ) ) ;
#4850 = CARTESIAN_POINT ( 'NONE',  ( 4.211140560182196957, 2.431303136016536470, -3.745885042887433514 ) ) ;
#4851 = ORIENTED_EDGE ( 'NONE', *, *, #5520, .T. ) ;
#4852 = CARTESIAN_POINT ( 'NONE',  ( 10.00000000000000000, -32.31183295104739273, -46.20417134726167063 ) ) ;
#4853 = ORIENTED_EDGE ( 'NONE', *, *, #15326, .T. ) ;
#4854 = DIRECTION ( 'NONE',  ( 0.000000000000000000, 0.000000000000000000, -1.000000000000000000 ) ) ;
#4855 = LINE ( 'NONE', #16280, #7693 ) ;
#4856 = AXIS2_PLACEMENT_3D ( 'NONE', #5492, #15491, #6814 ) ;
#4857 = ADVANCED_FACE ( 'NONE', ( #3916, #15528 ), #94, .T. ) ;
#4858 = CIRCLE ( 'NONE', #6990, 4.799999999999999822 ) ;
#4859 = ORIENTED_EDGE ( 'NONE', *, *, #17830, .F. ) ;
#4860 = DIRECTION ( 'NONE',  ( 0.01644736842105263414, -0.9998647328874152862, 0.000000000000000000 ) ) ;
#4861 = ORIENTED_EDGE ( 'NONE', *, *, #2606, .F. ) ;
#4862 = DIRECTION ( 'NONE',  ( 0.000000000000000000, 0.000000000000000000, 1.000000000000000000 ) ) ;
#4863 = CARTESIAN_POINT ( 'NONE',  ( 10.00000000000000000, -24.68609584167124282, -50.69000562871667626 ) ) ;
#4864 = CARTESIAN_POINT ( 'NONE',  ( 34.99999999999999289, 0.000000000000000000, 2.055000000000000160 ) ) ;
#4865 = CARTESIAN_POINT ( 'NONE',  ( 0.000000000000000000, 53.22058882792197210, 33.71303790549294632 ) ) ;
#4866 = LINE ( 'NONE', #776, #6562 ) ;
#4867 = ORIENTED_EDGE ( 'NONE', *, *, #8308, .F. ) ;
#4868 = CYLINDRICAL_SURFACE ( 'NONE', #4532, 26.24900000002624978 ) ;
#4869 = AXIS2_PLACEMENT_3D ( 'NONE', #5570, #8608, #6806 ) ;
#4870 = EDGE_CURVE ( 'NONE', #13797, #9771, #832, .T. ) ;
#4871 = SURFACE_SIDE_STYLE ('',( #4775 ) ) ;
#4872 = CARTESIAN_POINT ( 'NONE',  ( -10.00000000000000000, -5.120903701083534543E-13, -45.00000000000000000 ) ) ;
#4873 = EDGE_LOOP ( 'NONE', ( #13316, #6301, #13695, #17941 ) ) ;
#4874 = CONTEXT_DEPENDENT_SHAPE_REPRESENTATION ( #5134, #18798 ) ;
#4875 = ADVANCED_FACE ( 'NONE', ( #11705 ), #2668, .T. ) ;
#4876 = ORIENTED_EDGE ( 'NONE', *, *, #18327, .F. ) ;
#4877 = ORIENTED_EDGE ( 'NONE', *, *, #12760, .T. ) ;
#4878 = ADVANCED_FACE ( 'NONE', ( #4464 ), #9998, .F. ) ;
#4879 =( REPRESENTATION_RELATIONSHIP ('NONE','NONE', #11014, #2517 ) REPRESENTATION_RELATIONSHIP_WITH_TRANSFORMATION ( #6489 )SHAPE_REPRESENTATION_RELATIONSHIP( ) );
#4880 = EDGE_LOOP ( 'NONE', ( #3661, #8453, #14774, #3168 ) ) ;
#4881 = COLOUR_RGB ( '',0.8941176470588234615, 0.8941176470588234615, 0.8941176470588234615 ) ;
#4882 = FACE_OUTER_BOUND ( 'NONE', #16146, .T. ) ;
#4883 = CARTESIAN_POINT ( 'NONE',  ( -31.74999999999995737, 0.000000000000000000, 2.500000000000000444 ) ) ;
#4884 = ADVANCED_BREP_SHAPE_REPRESENTATION ( '', ( #3805, #8017 ), #7430 ) ;
#4885 = CARTESIAN_POINT ( 'NONE',  ( 0.000000000000000000, 0.000000000000000000, 0.000000000000000000 ) ) ;
#4886 = DIRECTION ( 'NONE',  ( 0.000000000000000000, 0.5877852522924742473, -0.8090169943749465631 ) ) ;
#4887 = DIRECTION ( 'NONE',  ( -0.000000000000000000, 1.000000000000000000, -0.000000000000000000 ) ) ;
#4888 = CARTESIAN_POINT ( 'NONE',  ( 11.25000000000000000, 29.90000000000000213, 0.000000000000000000 ) ) ;
#4889 = DIRECTION ( 'NONE',  ( 0.000000000000000000, 0.000000000000000000, -1.000000000000000000 ) ) ;
#4890 = DIRECTION ( 'NONE',  ( -1.000000000000000000, -0.000000000000000000, -0.000000000000000000 ) ) ;
#4891 = VERTEX_POINT ( 'NONE', #7126 ) ;
#4892 = CARTESIAN_POINT ( 'NONE',  ( 4.000000000000000000, -2.309401076758514915, -3.433295621305383349 ) ) ;
#4893 = EDGE_LOOP ( 'NONE', ( #6155, #8486 ) ) ;
#4894 = CARTESIAN_POINT ( 'NONE',  ( 0.000000000000000000, 0.000000000000000000, 0.000000000000000000 ) ) ;
#4895 = CARTESIAN_POINT ( 'NONE',  ( 0.6920835326022565237, 4.454600218803884459, -3.597382984111579862 ) ) ;
#4896 = CARTESIAN_POINT ( 'NONE',  ( -3.309651814758565180, -5.455921364805393026, 0.000000000000000000 ) ) ;
#4897 = VERTEX_POINT ( 'NONE', #1249 ) ;
#4898 = ORIENTED_EDGE ( 'NONE', *, *, #15760, .T. ) ;
#4899 = CARTESIAN_POINT ( 'NONE',  ( 10.00000000000000000, -22.07705612348849655, 14.19907017806860949 ) ) ;
#4900 = AXIS2_PLACEMENT_3D ( 'NONE', #10067, #17320, #18728 ) ;
#4901 = DIRECTION ( 'NONE',  ( 0.000000000000000000, 0.000000000000000000, 1.000000000000000000 ) ) ;
#4902 = CARTESIAN_POINT ( 'NONE',  ( 2.500000000000000000, 1.178949249685217415, 2.041999999999998483 ) ) ;
#4903 = ORIENTED_EDGE ( 'NONE', *, *, #12764, .F. ) ;
#4904 = CYLINDRICAL_SURFACE ( 'NONE', #9903, 24.00000000002399858 ) ;
#4905 = FACE_OUTER_BOUND ( 'NONE', #18171, .T. ) ;
#4906 = CARTESIAN_POINT ( 'NONE',  ( 0.000000000000000000, 0.000000000000000000, 56.24900000005625600 ) ) ;
#4907 = ORIENTED_EDGE ( 'NONE', *, *, #1568, .T. ) ;
#4908 = EDGE_CURVE ( 'NONE', #3106, #7239, #11472, .T. ) ;
#4910 = CYLINDRICAL_SURFACE ( 'NONE', #5821, 63.00000000006298961 ) ;
#4909 = CONICAL_SURFACE ( 'NONE', #13133, 4.000000000000000000, 0.8911886515913786111 ) ;
#4911 = EDGE_CURVE ( 'NONE', #16590, #14829, #7043, .T. ) ;
#4912 = ORIENTED_EDGE ( 'NONE', *, *, #11595, .T. ) ;
#4913 = CARTESIAN_POINT ( 'NONE',  ( 10.00000000000000000, 0.000000000000000000, 0.000000000000000000 ) ) ;
#4914 = ORIENTED_EDGE ( 'NONE', *, *, #6303, .F. ) ;
#4915 = AXIS2_PLACEMENT_3D ( 'NONE', #3834, #15462, #11556 ) ;
#4916 = CYLINDRICAL_SURFACE ( 'NONE', #4454, 33.00000000003299760 ) ;
#4917 = FACE_OUTER_BOUND ( 'NONE', #8910, .T. ) ;
#4918 = ORIENTED_EDGE ( 'NONE', *, *, #16108, .T. ) ;
#4919 = VERTEX_POINT ( 'NONE', #13139 ) ;
#4920 = DIRECTION ( 'NONE',  ( 0.000000000000000000, 0.1564344650402312575, -0.9876883405951376593 ) ) ;
#4921 = VERTEX_POINT ( 'NONE', #18756 ) ;
#4922 = FACE_OUTER_BOUND ( 'NONE', #10487, .T. ) ;
#4923 = EDGE_CURVE ( 'NONE', #18269, #16445, #9636, .T. ) ;
#4924 = AXIS2_PLACEMENT_3D ( 'NONE', #12575, #5617, #6962 ) ;
#4925 = FACE_OUTER_BOUND ( 'NONE', #15110, .T. ) ;
#4926 = ORIENTED_EDGE ( 'NONE', *, *, #12852, .T. ) ;
#4927 = EDGE_CURVE ( 'NONE', #8010, #11814, #12055, .T. ) ;
#4928 = ADVANCED_FACE ( 'NONE', ( #4096 ), #6956, .T. ) ;
#4929 = ORIENTED_EDGE ( 'NONE', *, *, #16784, .T. ) ;
#4930 = CARTESIAN_POINT ( 'NONE',  ( 0.000000000000000000, 34.13306034420251223, -44.70888270294124567 ) ) ;
#4931 = DIRECTION ( 'NONE',  ( 0.000000000000000000, 0.5877852522924684742, 0.8090169943749507819 ) ) ;
#4932 = CARTESIAN_POINT ( 'NONE',  ( -4.211140560182196957, -2.431303136016552013, -3.745885042887436178 ) ) ;
#4933 = ORIENTED_EDGE ( 'NONE', *, *, #1576, .T. ) ;
#4934 = DIRECTION ( 'NONE',  ( 0.000000000000000000, -1.000000000000000000, 0.000000000000000000 ) ) ;
#4935 = ADVANCED_FACE ( 'NONE', ( #11329 ), #15815, .T. ) ;
#4936 = CARTESIAN_POINT ( 'NONE',  ( 10.00000000000000000, 27.94286728106393269, 3.730438010304423013 ) ) ;
#4937 = DIRECTION ( 'NONE',  ( 1.000000000000000000, 0.000000000000000000, 0.000000000000000000 ) ) ;
#4938 = CYLINDRICAL_SURFACE ( 'NONE', #5368, 1.249999999999999778 ) ;
#4939 = ORIENTED_EDGE ( 'NONE', *, *, #14323, .F. ) ;
#4940 = ADVANCED_FACE ( 'NONE', ( #15716 ), #2853, .T. ) ;
#4941 = CARTESIAN_POINT ( 'NONE',  ( 10.00000000000000000, 47.29147401532012651, -41.62350880771872141 ) ) ;
#4942 = ORIENTED_EDGE ( 'NONE', *, *, #9430, .T. ) ;
#4943 = DIRECTION ( 'NONE',  ( 0.000000000000000000, 0.000000000000000000, 1.000000000000000000 ) ) ;
#4944 = CARTESIAN_POINT ( 'NONE',  ( 0.000000000000000000, -27.72801475327278453, -5.086963483077506787 ) ) ;
#4945 = EDGE_CURVE ( 'NONE', #8362, #5290, #8713, .T. ) ;
#4946 = ORIENTED_EDGE ( 'NONE', *, *, #10792, .T. ) ;
#4947 = AXIS2_PLACEMENT_3D ( 'NONE', #17112, #14056, #13857 ) ;
#4948 = AXIS2_PLACEMENT_3D ( 'NONE', #2592, #5353, #9643 ) ;
#4949 = ORIENTED_EDGE ( 'NONE', *, *, #7257, .F. ) ;
#4950 = LINE ( 'NONE', #18283, #9709 ) ;
#4951 = DIRECTION ( 'NONE',  ( 0.000000000000000000, 0.000000000000000000, 1.000000000000000000 ) ) ;
#4952 = CARTESIAN_POINT ( 'NONE',  ( -17.77999999999999758, 0.000000000000000000, 0.000000000000000000 ) ) ;
#4953 = CYLINDRICAL_SURFACE ( 'NONE', #15150, 56.24900000005625600 ) ;
#4954 = LINE ( 'NONE', #10758, #8098 ) ;
#4955 = ORIENTED_EDGE ( 'NONE', *, *, #10360, .F. ) ;
#4956 = DIRECTION ( 'NONE',  ( -0.9873298794253690946, 1.799126239882931805E-16, 0.1586811557617541224 ) ) ;
#4957 = EDGE_CURVE ( 'NONE', #243, #12652, #2764, .T. ) ;
#4958 = PRODUCT_DEFINITION_SHAPE ( 'NONE', 'NONE',  #15382 ) ;
#4959 = CARTESIAN_POINT ( 'NONE',  ( 4.249769933734876659, -30.10148593525447680, 0.000000000000000000 ) ) ;
#4960 = EDGE_LOOP ( 'NONE', ( #12556, #11023, #5095, #350 ) ) ;
#4961 = EDGE_LOOP ( 'NONE', ( #16232, #17313, #4799, #7973 ) ) ;
#4962 = VERTEX_POINT ( 'NONE', #4289 ) ;
#4963 = ORIENTED_EDGE ( 'NONE', *, *, #9468, .T. ) ;
#4964 = DIRECTION ( 'NONE',  ( -1.000000000000000000, 0.000000000000000000, -0.000000000000000000 ) ) ;
#4965 = CARTESIAN_POINT ( 'NONE',  ( -11.15000000000000391, 3.073863465859856794E-15, -25.10000000000000142 ) ) ;
#4966 = FACE_OUTER_BOUND ( 'NONE', #4980, .T. ) ;
#4967 = CARTESIAN_POINT ( 'NONE',  ( 10.00000000000000000, -9.514709542737069370, 24.46385708179980512 ) ) ;
#4968 = FILL_AREA_STYLE ('',( #13743 ) ) ;
#4969 = COLOUR_RGB ( '',0.8941176470588234615, 0.8941176470588234615, 0.8941176470588234615 ) ;
#4970 = CARTESIAN_POINT ( 'NONE',  ( 10.00000000000000000, 27.94286728106393269, 3.730438010304423013 ) ) ;
#4971 = FACE_OUTER_BOUND ( 'NONE', #7009, .T. ) ;
#4972 = CARTESIAN_POINT ( 'NONE',  ( -90.00000000009001155, 2.000000000000001776, 5.000000000000003553 ) ) ;
#4973 = ORIENTED_EDGE ( 'NONE', *, *, #1460, .T. ) ;
#4974 = CARTESIAN_POINT ( 'NONE',  ( 10.00000000000000000, 18.64666490672447097, -53.06836994729213330 ) ) ;
#4975 = VERTEX_POINT ( 'NONE', #10090 ) ;
#4976 = ADVANCED_FACE ( 'NONE', ( #15900 ), #15987, .T. ) ;
#4977 = CARTESIAN_POINT ( 'NONE',  ( 0.000000000000000000, 44.70888270294211253, -34.13306034420136825 ) ) ;
#4978 = CARTESIAN_POINT ( 'NONE',  ( -90.67999921423555065, 1.821459649775647449E-14, -4.751589320297106234 ) ) ;
#4979 = DIRECTION ( 'NONE',  ( -1.000000000000000000, -0.000000000000000000, -0.000000000000000000 ) ) ;
#4980 = EDGE_LOOP ( 'NONE', ( #10664, #14620, #12544, #5870 ) ) ;
#4981 = VERTEX_POINT ( 'NONE', #5803 ) ;
#4982 = CARTESIAN_POINT ( 'NONE',  ( -10.00000000000000000, 0.000000000000000000, 0.000000000000000000 ) ) ;
#4983 = DIRECTION ( 'NONE',  ( 0.000000000000000000, -1.000000000000000000, 0.000000000000000000 ) ) ;
#4984 = DIRECTION ( 'NONE',  ( -1.000000000000000000, 0.000000000000000000, 0.000000000000000000 ) ) ;
#4985 = EDGE_LOOP ( 'NONE', ( #4306, #5955 ) ) ;
#4986 = MECHANICAL_DESIGN_GEOMETRIC_PRESENTATION_REPRESENTATION (  '', ( #1957 ), #2255 ) ;
#4987 = EDGE_CURVE ( 'NONE', #16693, #6780, #8744, .T. ) ;
#4988 = DIRECTION ( 'NONE',  ( -1.000000000000000000, -0.000000000000000000, -0.000000000000000000 ) ) ;
#4989 = FACE_OUTER_BOUND ( 'NONE', #4073, .T. ) ;
#4990 = DIRECTION ( 'NONE',  ( -1.000000000000000000, -0.000000000000000000, 0.000000000000000000 ) ) ;
#4991 = ORIENTED_EDGE ( 'NONE', *, *, #13123, .F. ) ;
#4992 = PLANE ( 'NONE',  #2781 ) ;
#4993 = EDGE_CURVE ( 'NONE', #3333, #4781, #1796, .T. ) ;
#4994 = ORIENTED_EDGE ( 'NONE', *, *, #15173, .T. ) ;
#4995 = FACE_OUTER_BOUND ( 'NONE', #13965, .T. ) ;
#4996 = ORIENTED_EDGE ( 'NONE', *, *, #16337, .T. ) ;
#4997 = FACE_OUTER_BOUND ( 'NONE', #4354, .T. ) ;
#4998 = EDGE_LOOP ( 'NONE', ( #11032, #12903, #7537, #11564 ) ) ;
#4999 = ORIENTED_EDGE ( 'NONE', *, *, #9818, .T. ) ;
#5000 = VECTOR ( 'NONE', #16548, 1000.000000000000000 ) ;
#5001 = DIRECTION ( 'NONE',  ( 0.000000000000000000, 0.7071067811865440200, 0.7071067811865511255 ) ) ;
#5002 = ORIENTED_EDGE ( 'NONE', *, *, #2486, .F. ) ;
#5003 = FACE_OUTER_BOUND ( 'NONE', #2434, .T. ) ;
#5004 = PRODUCT_DEFINITION_FORMATION_WITH_SPECIFIED_SOURCE ( 'ANY', '', #9804, .NOT_KNOWN. ) ;
#5005 = CYLINDRICAL_SURFACE ( 'NONE', #3815, 24.00000000002400213 ) ;
#5006 = AXIS2_PLACEMENT_3D ( 'NONE', #18348, #11103, #5205 ) ;
#5008 = CIRCLE ( 'NONE', #14452, 24.00000000002400213 ) ;
#5007 = LINE ( 'NONE', #299, #10840 ) ;
#5009 = ORIENTED_EDGE ( 'NONE', *, *, #8767, .F. ) ;
#5010 = VERTEX_POINT ( 'NONE', #557 ) ;
#5011 = CARTESIAN_POINT ( 'NONE',  ( 2.836893136758676270, 3.208949435745843903, -3.505054077164911241 ) ) ;
#5012 = DIRECTION ( 'NONE',  ( 0.000000000000000000, 0.000000000000000000, 1.000000000000000000 ) ) ;
#5013 = CARTESIAN_POINT ( 'NONE',  ( 10.00000000000000000, 0.000000000000000000, 0.000000000000000000 ) ) ;
#5014 = ORIENTED_EDGE ( 'NONE', *, *, #12252, .F. ) ;
#5015 = LINE ( 'NONE', #18072, #16336 ) ;
#5016 = DIRECTION ( 'NONE',  ( 1.000000000000000000, 0.000000000000000000, 0.000000000000000000 ) ) ;
#5017 = CARTESIAN_POINT ( 'NONE',  ( 2.500000000000000000, 1.178949249685212974, -2.042000000000001148 ) ) ;
#5018 = CIRCLE ( 'NONE', #11473, 27.50000000000000000 ) ;
#5019 = CARTESIAN_POINT ( 'NONE',  ( 10.04305231718605285, -30.00000000000000000, -33.55933677959240669 ) ) ;
#5020 = EDGE_LOOP ( 'NONE', ( #12957, #11394, #2547, #4111 ) ) ;
#5021 = LINE ( 'NONE', #289, #5679 ) ;
#5022 = ORIENTED_EDGE ( 'NONE', *, *, #12782, .T. ) ;
#5023 = CARTESIAN_POINT ( 'NONE',  ( -4.101948962586059899, -2.368261337751176754, -3.681124513963741851 ) ) ;
#5024 = DIRECTION ( 'NONE',  ( 0.000000000000000000, 1.000000000000000000, 0.000000000000000000 ) ) ;
#5025 = CIRCLE ( 'NONE', #1395, 63.00000000006298961 ) ;
#5026 = EDGE_CURVE ( 'NONE', #2515, #18313, #16019, .T. ) ;
#5027 = EDGE_CURVE ( 'NONE', #11971, #6793, #12680, .T. ) ;
#5028 = ADVANCED_FACE ( 'NONE', ( #16462 ), #3415, .F. ) ;
#5029 = ADVANCED_FACE ( 'NONE', ( #1604, #6368 ), #9209, .F. ) ;
#5030 = CIRCLE ( 'NONE', #16006, 25.00000000000000000 ) ;
#5031 = CIRCLE ( 'NONE', #7781, 4.799999999999998934 ) ;
#5032 = ORIENTED_EDGE ( 'NONE', *, *, #9250, .F. ) ;
#5033 = EDGE_CURVE ( 'NONE', #6730, #13493, #14204, .T. ) ;
#5034 = CONICAL_SURFACE ( 'NONE', #12344, 2.041999999999999815, 1.047197551196591858 ) ;
#5035 = ORIENTED_EDGE ( 'NONE', *, *, #16675, .F. ) ;
#5036 = CARTESIAN_POINT ( 'NONE',  ( 4.999999999999999112, 4.007856633824268044, -62.87238730325617553 ) ) ;
#5037 = CARTESIAN_POINT ( 'NONE',  ( 4.000000000000000000, -2.471525695159793035, -3.686886880705770864 ) ) ;
#5038 = CIRCLE ( 'NONE', #194, 24.00000000002400213 ) ;
#5039 = DIRECTION ( 'NONE',  ( -1.000000000000000000, 0.000000000000000000, -0.000000000000000000 ) ) ;
#5040 = CARTESIAN_POINT ( 'NONE',  ( 0.000000000000000000, 13.79392154159224404, -61.47135697633764551 ) ) ;
#5041 =( BOUNDED_SURFACE ( )  B_SPLINE_SURFACE ( 3, 2, ( 
 ( #8288, #5037, #582 ),
 ( #13722, #5323, #2278 ),
 ( #15330, #6573, #7907 ),
 ( #18091, #18373, #2473 ),
 ( #6387, #3917, #16961 ),
 ( #12282, #673, #17999 ) ),
 .UNSPECIFIED., .F., .F., .F. ) 
 B_SPLINE_SURFACE_WITH_KNOTS ( ( 4, 2, 4 ),
 ( 3, 3 ),
 ( 0.02027065861071770947, 0.02273072267836921331, 0.02519078674602071716 ),
 ( 0.000000000000000000, 1.000000000000000000 ),
 .UNSPECIFIED. ) 
 GEOMETRIC_REPRESENTATION_ITEM ( )  RATIONAL_B_SPLINE_SURFACE ( (
 ( 1.000000000000000000, 0.8047781708337304885, 1.000000000000000000),
 ( 1.000000000000000000, 0.8123765190705307671, 1.000000000000000000),
 ( 1.000000000000000000, 0.8190656277163975707, 1.000000000000000000),
 ( 1.000000000000000000, 0.8192366903512159348, 1.000000000000000000),
 ( 1.000000000000000000, 0.8126138454302893610, 1.000000000000000000),
 ( 1.000000000000000000, 0.8047712246031417660, 1.000000000000000000) ) ) 
 REPRESENTATION_ITEM ( '' )  SURFACE ( )  );
#5042 = CARTESIAN_POINT ( 'NONE',  ( -26.29305231718568336, -26.50000000000000000, -21.75302069950551953 ) ) ;
#5043 = CARTESIAN_POINT ( 'NONE',  ( 10.00000000000000000, -55.83748330407401284, 16.18620087215011338 ) ) ;
#5044 = VERTEX_POINT ( 'NONE', #17889 ) ;
#5045 = CARTESIAN_POINT ( 'NONE',  ( -26.29305231718584324, -30.00000000000000000, 16.45302069950530566 ) ) ;
#5046 = FILL_AREA_STYLE_COLOUR ( '', #8635 ) ;
#5047 = CARTESIAN_POINT ( 'NONE',  ( -5.560781378645573980, 0.000000000000000000, -4.000000000000000000 ) ) ;
#5048 = ORIENTED_EDGE ( 'NONE', *, *, #8699, .F. ) ;
#5049 = CIRCLE ( 'NONE', #5678, 24.00000000002400569 ) ;
#5050 = CIRCLE ( 'NONE', #10823, 56.24900000005626310 ) ;
#5051 = ADVANCED_FACE ( 'NONE', ( #10551 ), #6078, .F. ) ;
#5052 = CONTEXT_DEPENDENT_SHAPE_REPRESENTATION ( #12676, #12106 ) ;
#5053 = AXIS2_PLACEMENT_3D ( 'NONE', #10773, #16594, #4121 ) ;
#5054 = ORIENTED_EDGE ( 'NONE', *, *, #4688, .F. ) ;
#5055 = CIRCLE ( 'NONE', #4759, 56.24900000005627021 ) ;
#5056 = CIRCLE ( 'NONE', #15717, 26.24900000002626044 ) ;
#5057 = EDGE_LOOP ( 'NONE', ( #9885, #9033, #15805, #18563 ) ) ;
#5058 = EDGE_CURVE ( 'NONE', #13093, #15064, #13609, .T. ) ;
#5059 = ORIENTED_EDGE ( 'NONE', *, *, #13913, .T. ) ;
#5060 = CYLINDRICAL_SURFACE ( 'NONE', #3859, 12.00000000001200462 ) ;
#5061 = CARTESIAN_POINT ( 'NONE',  ( -79.64793068852927149, -38.00000000000000000, 29.21039329588765554 ) ) ;
#5062 = CIRCLE ( 'NONE', #13901, 2.649999999999999467 ) ;
#5063 = AXIS2_PLACEMENT_3D ( 'NONE', #1781, #16167, #12162 ) ;
#5064 = DIRECTION ( 'NONE',  ( 0.000000000000000000, 0.000000000000000000, -1.000000000000000000 ) ) ;
#5065 = FACE_OUTER_BOUND ( 'NONE', #11763, .T. ) ;
#5067 = DIRECTION ( 'NONE',  ( -1.000000000000000000, 0.000000000000000000, 0.000000000000000000 ) ) ;
#5066 = VECTOR ( 'NONE', #14195, 1000.000000000000000 ) ;
#5068 = CARTESIAN_POINT ( 'NONE',  ( 10.00000000000000000, 0.000000000000000000, 0.000000000000000000 ) ) ;
#5069 = DIRECTION ( 'NONE',  ( -0.000000000000000000, -1.000000000000000000, 0.000000000000000000 ) ) ;
#5070 = TOROIDAL_SURFACE ( 'NONE', #9023, 25.10000000000000142, 0.09999999999999766020 ) ;
#5071 = LINE ( 'NONE', #7929, #15978 ) ;
#5072 = ORIENTED_EDGE ( 'NONE', *, *, #13101, .F. ) ;
#5073 = AXIS2_PLACEMENT_3D ( 'NONE', #5324, #15530, #2474 ) ;
#5074 = DIRECTION ( 'NONE',  ( -1.000000000000000000, 0.000000000000000000, 0.000000000000000000 ) ) ;
#5075 = ORIENTED_EDGE ( 'NONE', *, *, #379, .T. ) ;
#5076 = CARTESIAN_POINT ( 'NONE',  ( 2.500000000000000000, -2.357898499370432166, 3.035766082959412415E-15 ) ) ;
#5077 = DIRECTION ( 'NONE',  ( 0.9995004958639132076, 0.000000000000000000, 0.03160314490350067673 ) ) ;
#5078 = VERTEX_POINT ( 'NONE', #13421 ) ;
#5079 = ORIENTED_EDGE ( 'NONE', *, *, #16811, .T. ) ;
#5080 = CARTESIAN_POINT ( 'NONE',  ( 0.000000000000000000, 1.305124410222461284, 0.000000000000000000 ) ) ;
#5081 = CARTESIAN_POINT ( 'NONE',  ( 10.04305231718605285, -21.50000000000000000, -30.90933677959240811 ) ) ;
#5082 = CARTESIAN_POINT ( 'NONE',  ( 0.000000000000000000, 0.000000000000000000, 0.000000000000000000 ) ) ;
#5083 = VERTEX_POINT ( 'NONE', #4930 ) ;
#5084 = VECTOR ( 'NONE', #5463, 1000.000000000000000 ) ;
#5085 = AXIS2_PLACEMENT_3D ( 'NONE', #11017, #13885, #18557 ) ;
#5086 = AXIS2_PLACEMENT_3D ( 'NONE', #10988, #11079, #3861 ) ;
#5087 = CIRCLE ( 'NONE', #2663, 12.00000000001200284 ) ;
#5088 = EDGE_CURVE ( 'NONE', #845, #16631, #4190, .T. ) ;
#5089 = DIRECTION ( 'NONE',  ( 1.000000000000000000, 0.000000000000000000, -0.000000000000000000 ) ) ;
#5090 = FACE_BOUND ( 'NONE', #4468, .T. ) ;
#5091 = DIRECTION ( 'NONE',  ( 0.000000000000000000, 0.000000000000000000, 1.000000000000000000 ) ) ;
#5092 = EDGE_LOOP ( 'NONE', ( #3936, #11960, #11590, #12581 ) ) ;
#5093 = CARTESIAN_POINT ( 'NONE',  ( 10.00000000000000000, 14.27431201565524610, 29.75305054077477607 ) ) ;
#5094 = CIRCLE ( 'NONE', #5720, 4.250000000000000000 ) ;
#5095 = ORIENTED_EDGE ( 'NONE', *, *, #15882, .T. ) ;
#5096 = DIRECTION ( 'NONE',  ( -1.000000000000000000, -0.000000000000000000, 0.000000000000000000 ) ) ;
#5097 = EDGE_LOOP ( 'NONE', ( #10435, #3349, #4676, #5802 ) ) ;
#5098 = CIRCLE ( 'NONE', #16972, 2.055000000000000160 ) ;
#5099 = DIRECTION ( 'NONE',  ( 0.000000000000000000, -0.8090169943749402348, -0.5877852522924829071 ) ) ;
#5100 = CARTESIAN_POINT ( 'NONE',  ( 10.00000000000000000, 1.489278925039883239, -26.20671763660627107 ) ) ;
#5101 = CIRCLE ( 'NONE', #18185, 24.00000000002399858 ) ;
#5102 = ORIENTED_EDGE ( 'NONE', *, *, #12606, .F. ) ;
#5103 = VERTEX_POINT ( 'NONE', #7602 ) ;
#5104 = AXIS2_PLACEMENT_3D ( 'NONE', #15838, #13251, #8779 ) ;
#5105 = DIRECTION ( 'NONE',  ( 0.000000000000000000, 1.000000000000000000, -1.103561164596346103E-15 ) ) ;
#5106 = SURFACE_STYLE_FILL_AREA ( #1964 ) ;
#5107 = EDGE_CURVE ( 'NONE', #5250, #4319, #1736, .T. ) ;
#5108 = VERTEX_POINT ( 'NONE', #14845 ) ;
#5109 = DIRECTION ( 'NONE',  ( -1.000000000000000000, 0.000000000000000000, -0.000000000000000000 ) ) ;
#5110 = EDGE_CURVE ( 'NONE', #18521, #12641, #14214, .T. ) ;
#5111 = CIRCLE ( 'NONE', #9680, 26.24900000002624978 ) ;
#5112 = AXIS2_PLACEMENT_3D ( 'NONE', #313, #6112, #1829 ) ;
#5113 = CARTESIAN_POINT ( 'NONE',  ( 0.000000000000000000, -2.357898499370432166, 3.035766082959412415E-15 ) ) ;
#5114 = VECTOR ( 'NONE', #3533, 1000.000000000000000 ) ;
#5115 = DIRECTION ( 'NONE',  ( 0.000000000000000000, 0.000000000000000000, 1.000000000000000000 ) ) ;
#5116 = ORIENTED_EDGE ( 'NONE', *, *, #10964, .F. ) ;
#5117 = VERTEX_POINT ( 'NONE', #16177 ) ;
#5118 = DIRECTION ( 'NONE',  ( -1.000000000000000000, -0.000000000000000000, -0.000000000000000000 ) ) ;
#5119 = DIRECTION ( 'NONE',  ( 0.000000000000000000, 0.000000000000000000, 1.000000000000000000 ) ) ;
#5120 = CARTESIAN_POINT ( 'NONE',  ( 8.060728450267873768, -24.77235419320996357, -2.000000000000000000 ) ) ;
#5121 = ORIENTED_EDGE ( 'NONE', *, *, #17375, .T. ) ;
#5122 = CARTESIAN_POINT ( 'NONE',  ( -56.50000000009000445, -30.00000000000000000, 3.817814120399276590E-13 ) ) ;
#5123 = CYLINDRICAL_SURFACE ( 'NONE', #17011, 2.649999999999995914 ) ;
#5124 = DIRECTION ( 'NONE',  ( 1.000000000000000000, 0.000000000000000000, 0.000000000000000000 ) ) ;
#5125 = CIRCLE ( 'NONE', #15783, 63.00000000006298961 ) ;
#5126 = EDGE_LOOP ( 'NONE', ( #10625, #10506, #16849, #1585 ) ) ;
#5127 = ORIENTED_EDGE ( 'NONE', *, *, #4245, .T. ) ;
#5128 = DIRECTION ( 'NONE',  ( 0.000000000000000000, 0.000000000000000000, 1.000000000000000000 ) ) ;
#5129 = AXIS2_PLACEMENT_3D ( 'NONE', #5544, #17437, #12877 ) ;
#5130 = ORIENTED_EDGE ( 'NONE', *, *, #4365, .T. ) ;
#5131 = LINE ( 'NONE', #18366, #16692 ) ;
#5132 = DIRECTION ( 'NONE',  ( -1.000000000000000000, 0.000000000000000000, -0.000000000000000000 ) ) ;
#5133 = AXIS2_PLACEMENT_3D ( 'NONE', #12079, #3421, #9215 ) ;
#5134 =( REPRESENTATION_RELATIONSHIP ('NONE','NONE', #11014, #5670 ) REPRESENTATION_RELATIONSHIP_WITH_TRANSFORMATION ( #592 )SHAPE_REPRESENTATION_RELATIONSHIP( ) );
#5135 = VECTOR ( 'NONE', #3447, 1000.000000000000000 ) ;
#5136 = ORIENTED_EDGE ( 'NONE', *, *, #9335, .F. ) ;
#5137 = AXIS2_PLACEMENT_3D ( 'NONE', #1684, #5886, #10541 ) ;
#5138 = EDGE_LOOP ( 'NONE', ( #16498, #12689, #18685, #2355, #11119 ) ) ;
#5139 = DIRECTION ( 'NONE',  ( -0.000000000000000000, 1.000000000000000000, -0.000000000000000000 ) ) ;
#5140 = CARTESIAN_POINT ( 'NONE',  ( 10.00000000000000000, 0.000000000000000000, 0.000000000000000000 ) ) ;
#5141 = CARTESIAN_POINT ( 'NONE',  ( -79.64793068852927149, -30.00000000000000000, 31.86039329588764701 ) ) ;
#5142 = DIRECTION ( 'NONE',  ( 0.000000000000000000, 0.3090169943749410120, 0.9510565162951556406 ) ) ;
#5143 = EDGE_CURVE ( 'NONE', #6058, #7671, #527, .T. ) ;
#5144 = ADVANCED_FACE ( 'NONE', ( #8926 ), #14740, .T. ) ;
#5145 = CARTESIAN_POINT ( 'NONE',  ( -10.00000000000000000, 42.79754323328179311, -13.90576474687299680 ) ) ;
#5146 = DIRECTION ( 'NONE',  ( 0.000000000000000000, 0.000000000000000000, 1.000000000000000000 ) ) ;
#5147 = ORIENTED_EDGE ( 'NONE', *, *, #8422, .F. ) ;
#5148 = DIRECTION ( 'NONE',  ( 1.000000000000000000, 0.000000000000000000, 0.000000000000000000 ) ) ;
#5149 = EDGE_CURVE ( 'NONE', #3146, #16250, #6168, .T. ) ;
#5150 = DIRECTION ( 'NONE',  ( 0.000000000000000000, -1.000000000000000000, 1.103561164596346103E-15 ) ) ;
#5151 = VECTOR ( 'NONE', #10186, 1000.000000000000000 ) ;
#5152 = VERTEX_POINT ( 'NONE', #1881 ) ;
#5153 = AXIS2_PLACEMENT_3D ( 'NONE', #6699, #5067, #12501 ) ;
#5154 = EDGE_CURVE ( 'NONE', #7186, #11633, #7683, .T. ) ;
#5155 = ORIENTED_EDGE ( 'NONE', *, *, #15404, .F. ) ;
#5156 = EDGE_LOOP ( 'NONE', ( #12761, #17461, #17148, #4382 ) ) ;
#5157 = EDGE_CURVE ( 'NONE', #9088, #10404, #9039, .T. ) ;
#5158 = EDGE_LOOP ( 'NONE', ( #14022, #15387, #13424, #16248 ) ) ;
#5159 = LINE ( 'NONE', #9635, #11465 ) ;
#5160 = CARTESIAN_POINT ( 'NONE',  ( 10.04305231718605285, -26.50000000000000000, -30.90933677959240811 ) ) ;
#5161 = VECTOR ( 'NONE', #1382, 1000.000000000000000 ) ;
#5162 = CARTESIAN_POINT ( 'NONE',  ( -2.250000000000000000, -27.60846790388774608, 0.000000000000000000 ) ) ;
#5163 = DIRECTION ( 'NONE',  ( -1.000000000000000000, -0.000000000000000000, 0.000000000000000000 ) ) ;
#5164 = EDGE_CURVE ( 'NONE', #6521, #1178, #17268, .T. ) ;
#5165 = AXIS2_PLACEMENT_3D ( 'NONE', #9379, #1099, #14135 ) ;
#5166 = CARTESIAN_POINT ( 'NONE',  ( 10.00000000000000000, 34.13306034420185853, 44.70888270294173594 ) ) ;
#5167 = EDGE_CURVE ( 'NONE', #8307, #8867, #10250, .T. ) ;
#5168 = CARTESIAN_POINT ( 'NONE',  ( 0.000000000000000000, 0.000000000000000000, 0.000000000000000000 ) ) ;
#5169 = DIRECTION ( 'NONE',  ( 0.000000000000000000, 0.000000000000000000, 1.000000000000000000 ) ) ;
#5170 = CARTESIAN_POINT ( 'NONE',  ( 10.00000000000000000, 24.33982105418901298, 50.71018745830453156 ) ) ;
#5171 = VERTEX_POINT ( 'NONE', #184 ) ;
#5172 = DIRECTION ( 'NONE',  ( -1.000000000000000000, -0.000000000000000000, 0.000000000000000000 ) ) ;
#5173 = ORIENTED_EDGE ( 'NONE', *, *, #3198, .T. ) ;
#5174 = EDGE_CURVE ( 'NONE', #9048, #8021, #3578, .T. ) ;
#5175 = DIRECTION ( 'NONE',  ( -0.000000000000000000, 0.000000000000000000, -1.000000000000000000 ) ) ;
#5176 = DIRECTION ( 'NONE',  ( 1.000000000000000000, 0.000000000000000000, 0.000000000000000000 ) ) ;
#5177 = ORIENTED_EDGE ( 'NONE', *, *, #17207, .F. ) ;
#5178 = ORIENTED_EDGE ( 'NONE', *, *, #4028, .T. ) ;
#5179 = EDGE_CURVE ( 'NONE', #298, #4661, #843, .T. ) ;
#5180 = DIRECTION ( 'NONE',  ( 0.000000000000000000, 0.3090169943749480619, -0.9510565162951533091 ) ) ;
#5181 = DIRECTION ( 'NONE',  ( 1.892183365217141223E-17, -1.000000000000000000, -5.823541592445440773E-17 ) ) ;
#5182 = CARTESIAN_POINT ( 'NONE',  ( 1.411581201560190495E-15, 4.862606272033091592, -3.745885042887436622 ) ) ;
#5183 = ORIENTED_EDGE ( 'NONE', *, *, #9341, .T. ) ;
#5184 = AXIS2_PLACEMENT_3D ( 'NONE', #12717, #1377, #12614 ) ;
#5185 = CIRCLE ( 'NONE', #3672, 0.09999999999999939493 ) ;
#5186 = CARTESIAN_POINT ( 'NONE',  ( 10.00000000000000000, -55.83748330407401284, -7.813799127873885197 ) ) ;
#5187 = DIRECTION ( 'NONE',  ( 0.000000000000000000, 0.000000000000000000, 1.000000000000000000 ) ) ;
#5188 = CARTESIAN_POINT ( 'NONE',  ( 4.999999999999999112, 62.72529079327807011, 5.876895005582658982 ) ) ;
#5189 = ORIENTED_EDGE ( 'NONE', *, *, #2583, .F. ) ;
#5190 = DIRECTION ( 'NONE',  ( 1.000000000000000000, 0.000000000000000000, 0.000000000000000000 ) ) ;
#5191 = EDGE_LOOP ( 'NONE', ( #12397, #11295, #13327, #3847 ) ) ;
#5192 = CARTESIAN_POINT ( 'NONE',  ( -90.00000000009001155, -38.00000000000000000, -1.301042606982603940E-15 ) ) ;
#5193 = ORIENTED_EDGE ( 'NONE', *, *, #17293, .F. ) ;
#5194 = VECTOR ( 'NONE', #13525, 1000.000000000000000 ) ;
#5195 = DIRECTION ( 'NONE',  ( -0.000000000000000000, -1.000000000000000000, -0.000000000000000000 ) ) ;
#5196 = CARTESIAN_POINT ( 'NONE',  ( 10.00000000000000000, -38.81885513159959800, -40.70683587897998734 ) ) ;
#5197 = DIRECTION ( 'NONE',  ( 0.1586811557617541502, -1.606889522083424400E-16, 0.9873298794253692057 ) ) ;
#5198 = EDGE_LOOP ( 'NONE', ( #3451, #690, #8535, #5749 ) ) ;
#5199 = ORIENTED_EDGE ( 'NONE', *, *, #16704, .T. ) ;
#5200 = EDGE_CURVE ( 'NONE', #4436, #7904, #11487, .T. ) ;
#5201 = DIRECTION ( 'NONE',  ( -0.000000000000000000, 1.000000000000000000, -0.000000000000000000 ) ) ;
#5202 = ORIENTED_EDGE ( 'NONE', *, *, #3545, .T. ) ;
#5203 = CARTESIAN_POINT ( 'NONE',  ( -2.250000000000000000, -27.60846790388774608, -2.000000000000000000 ) ) ;
#5204 = CIRCLE ( 'NONE', #1569, 33.00000000003299760 ) ;
#5205 = DIRECTION ( 'NONE',  ( 0.000000000000000000, 0.000000000000000000, -1.000000000000000000 ) ) ;
#5206 = CARTESIAN_POINT ( 'NONE',  ( 0.000000000000000000, -53.29895248911662264, -18.38754094778296277 ) ) ;
#5207 = EDGE_LOOP ( 'NONE', ( #10879, #7424, #17278, #10605 ) ) ;
#5208 = CARTESIAN_POINT ( 'NONE',  ( 5.000000000000000000, 15.68049343255996320, 29.03656532225569009 ) ) ;
#5209 = EDGE_LOOP ( 'NONE', ( #9289, #4867 ) ) ;
#5210 = CARTESIAN_POINT ( 'NONE',  ( 3.540020015735602765, 2.810662092924382627, -3.602146406945867962 ) ) ;
#5211 = CARTESIAN_POINT ( 'NONE',  ( 0.000000000000000000, 15.00000000000000000, 0.000000000000000000 ) ) ;
#5212 = DIRECTION ( 'NONE',  ( 0.9938152567191714803, 0.000000000000000000, -0.1110460963393456596 ) ) ;
#5213 = ORIENTED_EDGE ( 'NONE', *, *, #2238, .F. ) ;
#5214 = CARTESIAN_POINT ( 'NONE',  ( 1.567478505476134606E-15, 4.618802153517012066, -3.433295621305382905 ) ) ;
#5215 = ORIENTED_EDGE ( 'NONE', *, *, #15890, .F. ) ;
#5216 = CARTESIAN_POINT ( 'NONE',  ( 5.000000000000000000, -22.76987570971509811, -23.88582760061506249 ) ) ;
#5217 = CYLINDRICAL_SURFACE ( 'NONE', #14992, 23.50000000000000355 ) ;
#5218 = ORIENTED_EDGE ( 'NONE', *, *, #12446, .T. ) ;
#5219 = ORIENTED_EDGE ( 'NONE', *, *, #10170, .F. ) ;
#5220 = ADVANCED_FACE ( 'NONE', ( #5983 ), #8746, .T. ) ;
#5221 = ORIENTED_EDGE ( 'NONE', *, *, #11983, .T. ) ;
#5222 = DIRECTION ( 'NONE',  ( 0.000000000000000000, 0.000000000000000000, 1.000000000000000000 ) ) ;
#5223 = DIRECTION ( 'NONE',  ( -1.000000000000000000, 0.000000000000000000, 0.000000000000000000 ) ) ;
#5224 = AXIS2_PLACEMENT_3D ( 'NONE', #17175, #7068, #4126 ) ;
#5225 = VECTOR ( 'NONE', #5429, 1000.000000000000000 ) ;
#5226 = EDGE_CURVE ( 'NONE', #18793, #4272, #2349, .T. ) ;
#5227 = ORIENTED_EDGE ( 'NONE', *, *, #10187, .T. ) ;
#5228 = AXIS2_PLACEMENT_3D ( 'NONE', #1326, #8901, #16432 ) ;
#5229 = ORIENTED_EDGE ( 'NONE', *, *, #16930, .T. ) ;
#5230 = DIRECTION ( 'NONE',  ( -1.000000000000000000, 0.000000000000000000, 0.000000000000000000 ) ) ;
#5231 = CARTESIAN_POINT ( 'NONE',  ( 0.000000000000000000, 0.000000000000000000, 0.000000000000000000 ) ) ;
#5232 = DIRECTION ( 'NONE',  ( 0.000000000000000000, 0.000000000000000000, -1.000000000000000000 ) ) ;
#5233 = DIRECTION ( 'NONE',  ( 0.000000000000000000, 0.000000000000000000, -1.000000000000000000 ) ) ;
#5234 = EDGE_CURVE ( 'NONE', #9593, #5722, #11707, .T. ) ;
#5235 = CIRCLE ( 'NONE', #981, 0.7499999999999997780 ) ;
#5236 = DIRECTION ( 'NONE',  ( -1.000000000000000000, -0.000000000000000000, -0.000000000000000000 ) ) ;
#5237 = CARTESIAN_POINT ( 'NONE',  ( 2.500000000000000000, 2.500728763858895382E-16, -2.041999999999999815 ) ) ;
#5238 = CARTESIAN_POINT ( 'NONE',  ( 0.000000000000000000, 0.000000000000000000, -4.974599999999998801 ) ) ;
#5239 = EDGE_LOOP ( 'NONE', ( #9497, #12150, #1383, #11987 ) ) ;
#5240 = DIRECTION ( 'NONE',  ( 0.000000000000000000, -1.000000000000000000, 0.000000000000000000 ) ) ;
#5241 = CARTESIAN_POINT ( 'NONE',  ( 0.000000000000000000, 32.11449294037271329, -54.20017844242479299 ) ) ;
#5242 = CARTESIAN_POINT ( 'NONE',  ( 10.04305231718579705, -30.00000000000000000, 30.90933677959249337 ) ) ;
#5243 = ITEM_DEFINED_TRANSFORMATION ( 'NONE', 'NONE', #7445,  #8017 ) ;
#5244 = ORIENTED_EDGE ( 'NONE', *, *, #6974, .F. ) ;
#5245 = CIRCLE ( 'NONE', #18013, 56.24900000005625600 ) ;
#5246 = EDGE_CURVE ( 'NONE', #1734, #4317, #3047, .T. ) ;
#5247 = VERTEX_POINT ( 'NONE', #10277 ) ;
#5248 = CIRCLE ( 'NONE', #8894, 24.00000000002399858 ) ;
#5249 = CIRCLE ( 'NONE', #4058, 56.24900000005625600 ) ;
#5250 = VERTEX_POINT ( 'NONE', #17514 ) ;
#5251 = CARTESIAN_POINT ( 'NONE',  ( 10.00000000000000000, 0.000000000000000000, 0.000000000000000000 ) ) ;
#5252 = FACE_OUTER_BOUND ( 'NONE', #2009, .T. ) ;
#5253 = CARTESIAN_POINT ( 'NONE',  ( 10.00000000000000000, -1.017308535511979972, -56.37237871411034718 ) ) ;
#5254 = CARTESIAN_POINT ( 'NONE',  ( 10.00000000000000000, 62.87238730325621106, 4.007856633823605463 ) ) ;
#5255 = CARTESIAN_POINT ( 'NONE',  ( 0.000000000000000000, 0.000000000000000000, 0.000000000000000000 ) ) ;
#5256 = DIRECTION ( 'NONE',  ( 0.000000000000000000, 0.7071067811865486830, -0.7071067811865463515 ) ) ;
#5257 = DIRECTION ( 'NONE',  ( 1.000000000000000000, 0.000000000000000000, 0.000000000000000000 ) ) ;
#5258 = DIRECTION ( 'NONE',  ( 1.000000000000000000, 0.000000000000000000, 0.000000000000000000 ) ) ;
#5259 = EDGE_LOOP ( 'NONE', ( #17923, #5075 ) ) ;
#5260 = LINE ( 'NONE', #10778, #16080 ) ;
#5261 = ORIENTED_EDGE ( 'NONE', *, *, #1559, .T. ) ;
#5262 = AXIS2_PLACEMENT_3D ( 'NONE', #6725, #5388, #11290 ) ;
#5263 = FACE_OUTER_BOUND ( 'NONE', #5313, .T. ) ;
#5264 = DIRECTION ( 'NONE',  ( -1.000000000000000000, -0.000000000000000000, -0.000000000000000000 ) ) ;
#5265 = ORIENTED_EDGE ( 'NONE', *, *, #11324, .T. ) ;
#5266 = ORIENTED_EDGE ( 'NONE', *, *, #15758, .T. ) ;
#5267 = AXIS2_PLACEMENT_3D ( 'NONE', #7797, #1811, #9317 ) ;
#5268 = DIRECTION ( 'NONE',  ( 0.000000000000000000, -0.3090169943749548898, 0.9510565162951511997 ) ) ;
#5269 = CARTESIAN_POINT ( 'NONE',  ( 10.00000000000000000, 0.000000000000000000, 0.000000000000000000 ) ) ;
#5270 = VERTEX_POINT ( 'NONE', #12695 ) ;
#5271 = B_SPLINE_CURVE_WITH_KNOTS ( 'NONE', 3,
 ( #11890, #2957, #14468, #2860, #7234, #16470, #9415, #10829 ),
 .UNSPECIFIED., .F., .F.,
 ( 4, 2, 2, 4 ),
 ( 2.465131517390770070E-07, 0.001183067374689869946, 0.001774477805458935659, 0.002365888236228001588 ),
 .UNSPECIFIED. ) ;
#5272 = EDGE_CURVE ( 'NONE', #10680, #14902, #987, .T. ) ;
#5273 = ADVANCED_FACE ( 'NONE', ( #2855 ), #11265, .T. ) ;
#5274 = EDGE_CURVE ( 'NONE', #13860, #5078, #11157, .T. ) ;
#5275 = AXIS2_PLACEMENT_3D ( 'NONE', #10333, #4523, #7460 ) ;
#5276 = CARTESIAN_POINT ( 'NONE',  ( 13.90576474687299680, 10.00000000000000000, 40.14754323328178742 ) ) ;
#5277 = EDGE_CURVE ( 'NONE', #7753, #12641, #13916, .T. ) ;
#5278 = CARTESIAN_POINT ( 'NONE',  ( 10.00000000000000000, 31.97297851452492168, -46.27827401617368963 ) ) ;
#5279 = CARTESIAN_POINT ( 'NONE',  ( 10.00000000000000000, 26.71881558261730660, 49.49802920186232313 ) ) ;
#5280 = DIRECTION ( 'NONE',  ( -1.000000000000000000, 0.000000000000000000, 0.000000000000000000 ) ) ;
#5281 = EDGE_CURVE ( 'NONE', #13753, #15698, #5708, .T. ) ;
#5282 = VERTEX_POINT ( 'NONE', #12591 ) ;
#5283 = DIRECTION ( 'NONE',  ( -1.000000000000000000, -0.000000000000000000, -0.000000000000000000 ) ) ;
#5284 = ORIENTED_EDGE ( 'NONE', *, *, #16542, .F. ) ;
#5285 = ADVANCED_FACE ( 'NONE', ( #5805 ), #1423, .T. ) ;
#5286 = FACE_OUTER_BOUND ( 'NONE', #18515, .T. ) ;
#5287 = CARTESIAN_POINT ( 'NONE',  ( 10.00000000000000000, -34.13306034420217827, 44.70888270294149436 ) ) ;
#5288 = CARTESIAN_POINT ( 'NONE',  ( 5.384454397937118664, 0.000000000000000000, -5.000000000000000000 ) ) ;
#5289 = ORIENTED_EDGE ( 'NONE', *, *, #3646, .F. ) ;
#5290 = VERTEX_POINT ( 'NONE', #11160 ) ;
#5291 = DIRECTION ( 'NONE',  ( 0.000000000000000000, 0.000000000000000000, -1.000000000000000000 ) ) ;
#5292 = CIRCLE ( 'NONE', #6498, 24.00000000002399858 ) ;
#5293 = ORIENTED_EDGE ( 'NONE', *, *, #4813, .F. ) ;
#5294 = CARTESIAN_POINT ( 'NONE',  ( 10.00000000000000000, 55.83748330407408389, -7.813799127873475747 ) ) ;
#5295 = EDGE_CURVE ( 'NONE', #13893, #484, #2049, .T. ) ;
#5296 = DIRECTION ( 'NONE',  ( 0.000000000000000000, 0.000000000000000000, 1.000000000000000000 ) ) ;
#5297 = DIRECTION ( 'NONE',  ( 1.000000000000000000, -0.000000000000000000, -0.000000000000000000 ) ) ;
#5298 = ADVANCED_FACE ( 'NONE', ( #15989 ), #14562, .T. ) ;
#5299 = VERTEX_POINT ( 'NONE', #16464 ) ;
#5300 = CARTESIAN_POINT ( 'NONE',  ( -2.000000000000002665, -3.464101615137770374, -3.142992957459237680 ) ) ;
#5301 = EDGE_LOOP ( 'NONE', ( #18311, #7953 ) ) ;
#5302 = DIRECTION ( 'NONE',  ( 0.000000000000000000, 0.000000000000000000, 1.000000000000000000 ) ) ;
#5303 = LINE ( 'NONE', #11111, #16882 ) ;
#5304 = DIRECTION ( 'NONE',  ( 0.000000000000000000, 0.000000000000000000, 1.000000000000000000 ) ) ;
#5305 = EDGE_LOOP ( 'NONE', ( #825, #441, #17003, #4366 ) ) ;
#5306 = DIRECTION ( 'NONE',  ( 0.000000000000000000, -1.000000000000000000, 1.287488025362403787E-15 ) ) ;
#5307 = ORIENTED_EDGE ( 'NONE', *, *, #14012, .T. ) ;
#5308 = DIRECTION ( 'NONE',  ( -1.000000000000000000, -0.000000000000000000, 0.000000000000000000 ) ) ;
#5309 = CYLINDRICAL_SURFACE ( 'NONE', #12236, 30.00000000000000711 ) ;
#5310 = VERTEX_POINT ( 'NONE', #3611 ) ;
#5311 = ORIENTED_EDGE ( 'NONE', *, *, #12606, .T. ) ;
#5312 = DIRECTION ( 'NONE',  ( 0.000000000000000000, 0.000000000000000000, 1.000000000000000000 ) ) ;
#5313 = EDGE_LOOP ( 'NONE', ( #14084, #999, #17764, #4134 ) ) ;
#5314 = CARTESIAN_POINT ( 'NONE',  ( 10.04305231718605285, -26.50000000000000000, -30.90933677959240811 ) ) ;
#5315 = CARTESIAN_POINT ( 'NONE',  ( -11.15000000000000391, 0.000000000000000000, 25.00000000000000000 ) ) ;
#5316 = AXIS2_PLACEMENT_3D ( 'NONE', #16520, #3384, #12314 ) ;
#5317 = AXIS2_PLACEMENT_3D ( 'NONE', #9493, #5500, #17034 ) ;
#5318 = AXIS2_PLACEMENT_3D ( 'NONE', #15031, #3700, #18354 ) ;
#5319 = EDGE_CURVE ( 'NONE', #12639, #18552, #1643, .T. ) ;
#5320 = ORIENTED_EDGE ( 'NONE', *, *, #11687, .T. ) ;
#5321 = VERTEX_POINT ( 'NONE', #279 ) ;
#5322 = CARTESIAN_POINT ( 'NONE',  ( 0.000000000000000000, 0.000000000000000000, 0.000000000000000000 ) ) ;
#5323 = CARTESIAN_POINT ( 'NONE',  ( 4.000000000000000000, -1.677850389431204459, -3.535268758346977513 ) ) ;
#5324 = CARTESIAN_POINT ( 'NONE',  ( 10.00000000000000000, -40.58063702438316511, -39.14194549634407139 ) ) ;
#5325 = CARTESIAN_POINT ( 'NONE',  ( 0.000000000000000000, 0.000000000000000000, 0.000000000000000000 ) ) ;
#5326 = PRODUCT_DEFINITION_FORMATION_WITH_SPECIFIED_SOURCE ( 'ANY', '', #17887, .NOT_KNOWN. ) ;
#5327 = CIRCLE ( 'NONE', #3109, 63.00000000006298961 ) ;
#5328 = DIRECTION ( 'NONE',  ( 0.000000000000000000, 0.000000000000000000, 1.000000000000000000 ) ) ;
#5329 = CARTESIAN_POINT ( 'NONE',  ( 10.00000000000000000, 18.38754094778314752, -53.29895248911656580 ) ) ;
#5330 = CIRCLE ( 'NONE', #9281, 12.00000000001200817 ) ;
#5331 = DIRECTION ( 'NONE',  ( 0.000000000000000000, 0.000000000000000000, 1.000000000000000000 ) ) ;
#5332 = ORIENTED_EDGE ( 'NONE', *, *, #5959, .F. ) ;
#5333 = DIRECTION ( 'NONE',  ( -1.000000000000000000, 0.000000000000000000, -0.000000000000000000 ) ) ;
#5334 = AXIS2_PLACEMENT_3D ( 'NONE', #12216, #18025, #9358 ) ;
#5335 = DIRECTION ( 'NONE',  ( 0.000000000000000000, 0.000000000000000000, 1.000000000000000000 ) ) ;
#5336 = CARTESIAN_POINT ( 'NONE',  ( 10.00000000000000000, 13.40641754777700534, -24.79895094899245933 ) ) ;
#5337 = CARTESIAN_POINT ( 'NONE',  ( 0.000000000000000000, 13.40641754777665717, 24.79895094899264052 ) ) ;
#5338 = EDGE_CURVE ( 'NONE', #14293, #3106, #15438, .T. ) ;
#5339 = CONTEXT_DEPENDENT_SHAPE_REPRESENTATION ( #11340, #10125 ) ;
#5340 = ORIENTED_EDGE ( 'NONE', *, *, #16920, .T. ) ;
#5341 = VECTOR ( 'NONE', #8711, 1000.000000000000000 ) ;
#5342 = EDGE_CURVE ( 'NONE', #13131, #15635, #6292, .T. ) ;
#5343 = ORIENTED_EDGE ( 'NONE', *, *, #2646, .T. ) ;
#5344 = AXIS2_PLACEMENT_3D ( 'NONE', #12610, #3962, #3674 ) ;
#5345 = CIRCLE ( 'NONE', #8980, 0.7500000000000000000 ) ;
#5346 = EDGE_LOOP ( 'NONE', ( #18067, #15296, #1766, #1034, #9961 ) ) ;
#5347 = DIRECTION ( 'NONE',  ( 0.000000000000000000, -0.5877852522924801315, 0.8090169943749422332 ) ) ;
#5348 = DIRECTION ( 'NONE',  ( 0.000000000000000000, 0.000000000000000000, 1.000000000000000000 ) ) ;
#5349 = LINE ( 'NONE', #10873, #14251 ) ;
#5350 = DIRECTION ( 'NONE',  ( -1.000000000000000000, 0.000000000000000000, -0.000000000000000000 ) ) ;
#5351 = CARTESIAN_POINT ( 'NONE',  ( 0.000000000000000000, 0.000000000000000000, 0.000000000000000000 ) ) ;
#5352 = CARTESIAN_POINT ( 'NONE',  ( 10.00000000000000000, 18.64666490672371424, 53.06836994729241042 ) ) ;
#5353 = DIRECTION ( 'NONE',  ( 0.000000000000000000, -1.000000000000000000, 0.000000000000000000 ) ) ;
#5354 = AXIS2_PLACEMENT_3D ( 'NONE', #10980, #18318, #5268 ) ;
#5355 = CARTESIAN_POINT ( 'NONE',  ( 0.000000000000000000, -40.19788616105574164, -48.50907078259425731 ) ) ;
#5356 = ADVANCED_BREP_SHAPE_REPRESENTATION ( '', ( #9701, #8017 ), #737 ) ;
#5357 = ORIENTED_EDGE ( 'NONE', *, *, #9641, .F. ) ;
#5358 = DIRECTION ( 'NONE',  ( -1.000000000000000000, -0.000000000000000000, -0.000000000000000000 ) ) ;
#5359 = CIRCLE ( 'NONE', #8089, 63.00000000006298961 ) ;
#5360 = VERTEX_POINT ( 'NONE', #656 ) ;
#5361 = AXIS2_PLACEMENT_3D ( 'NONE', #18687, #985, #9834 ) ;
#5362 = CARTESIAN_POINT ( 'NONE',  ( -10.00000000000000000, 26.45033635316149301, 33.75576474687247241 ) ) ;
#5363 = LINE ( 'NONE', #8327, #17575 ) ;
#5364 = ORIENTED_EDGE ( 'NONE', *, *, #13913, .F. ) ;
#5365 = CIRCLE ( 'NONE', #16947, 2.649999999999999467 ) ;
#5366 = EDGE_LOOP ( 'NONE', ( #5958, #10697, #12416, #12600, #17716, #8819 ) ) ;
#5367 = CIRCLE ( 'NONE', #3236, 26.24900000002624978 ) ;
#5368 = AXIS2_PLACEMENT_3D ( 'NONE', #12270, #461, #1888 ) ;
#5369 = CARTESIAN_POINT ( 'NONE',  ( -4.000000000000000000, -2.309401076758515803, -0.4999999999999995559 ) ) ;
#5370 = CARTESIAN_POINT ( 'NONE',  ( -117.1020693116506379, -43.00000000000000000, -19.69080595179801207 ) ) ;
#5371 = CARTESIAN_POINT ( 'NONE',  ( 0.000000000000000000, 10.00000000000000000, 0.000000000000000000 ) ) ;
#5372 = EDGE_LOOP ( 'NONE', ( #12348, #5568, #17442, #3351 ) ) ;
#5373 = AXIS2_PLACEMENT_3D ( 'NONE', #1420, #13048, #7 ) ;
#5374 = AXIS2_PLACEMENT_3D ( 'NONE', #3342, #6180, #9137 ) ;
#5375 = DIRECTION ( 'NONE',  ( -1.000000000000000000, 0.000000000000000000, -0.000000000000000000 ) ) ;
#5376 = CARTESIAN_POINT ( 'NONE',  ( -26.29305231718584324, -26.50000000000000000, 21.75302069950530637 ) ) ;
#5377 = VECTOR ( 'NONE', #16698, 1000.000000000000000 ) ;
#5378 = VECTOR ( 'NONE', #5567, 1000.000000000000000 ) ;
#5379 = DIRECTION ( 'NONE',  ( 0.000000000000000000, -0.4999999999999993339, 0.8660254037844390407 ) ) ;
#5380 = FACE_OUTER_BOUND ( 'NONE', #7190, .T. ) ;
#5381 = UNCERTAINTY_MEASURE_WITH_UNIT (LENGTH_MEASURE( 1.000000000000000082E-05 ), #13730, 'distance_accuracy_value', 'NONE');
#5382 = FACE_OUTER_BOUND ( 'NONE', #3412, .T. ) ;
#5383 = ORIENTED_EDGE ( 'NONE', *, *, #10220, .T. ) ;
#5384 = ADVANCED_FACE ( 'NONE', ( #1694 ), #7508, .T. ) ;
#5385 = EDGE_CURVE ( 'NONE', #17330, #7275, #559, .T. ) ;
#5386 = EDGE_CURVE ( 'NONE', #9315, #2222, #2084, .T. ) ;
#5387 = CARTESIAN_POINT ( 'NONE',  ( 0.000000000000000000, 0.000000000000000000, -0.2800830152838844622 ) ) ;
#5388 = DIRECTION ( 'NONE',  ( 0.000000000000000000, -1.000000000000000000, 0.000000000000000000 ) ) ;
#5389 = LINE ( 'NONE', #14057, #17353 ) ;
#5390 = AXIS2_PLACEMENT_3D ( 'NONE', #1076, #10368, #16089 ) ;
#5391 = VERTEX_POINT ( 'NONE', #15032 ) ;
#5392 = ORIENTED_EDGE ( 'NONE', *, *, #13718, .T. ) ;
#5393 = DIRECTION ( 'NONE',  ( 0.000000000000000000, 0.000000000000000000, 1.000000000000000000 ) ) ;
#5394 = CIRCLE ( 'NONE', #16035, 23.50000000000000355 ) ;
#5395 = EDGE_CURVE ( 'NONE', #13122, #1501, #13423, .T. ) ;
#5396 = EDGE_LOOP ( 'NONE', ( #18537, #8573, #748, #14153 ) ) ;
#5397 = CARTESIAN_POINT ( 'NONE',  ( -11.25000000000000355, 3.306546357697854128E-15, 27.00000000000000355 ) ) ;
#5398 = CIRCLE ( 'NONE', #7503, 24.00000000002400213 ) ;
#5399 = AXIS2_PLACEMENT_3D ( 'NONE', #15311, #7886, #5302 ) ;
#5400 = EDGE_CURVE ( 'NONE', #10719, #6939, #15126, .T. ) ;
#5401 = CARTESIAN_POINT ( 'NONE',  ( 20.55500000000001748, 0.000000000000000000, 2.500000000000000888 ) ) ;
#5402 = EDGE_CURVE ( 'NONE', #9858, #3146, #1147, .T. ) ;
#5403 = AXIS2_PLACEMENT_3D ( 'NONE', #18355, #14166, #6936 ) ;
#5404 = CARTESIAN_POINT ( 'NONE',  ( 10.00000000000000000, -40.19788616105643797, 48.50907078259367466 ) ) ;
#5405 = ORIENTED_EDGE ( 'NONE', *, *, #5768, .F. ) ;
#5406 =( NAMED_UNIT ( * ) SI_UNIT ( $, .STERADIAN. ) SOLID_ANGLE_UNIT ( ) );
#5407 = CIRCLE ( 'NONE', #10566, 56.24900000005626310 ) ;
#5408 = VECTOR ( 'NONE', #18140, 1000.000000000000000 ) ;
#5409 = ORIENTED_EDGE ( 'NONE', *, *, #5272, .F. ) ;
#5411 = DIRECTION ( 'NONE',  ( 0.9995004958639132076, 0.000000000000000000, 0.03160314490350067673 ) ) ;
#5410 = PRODUCT_DEFINITION_CONTEXT ( 'detailed design', #11448, 'design' ) ;
#5412 = CIRCLE ( 'NONE', #12091, 26.24900000002624978 ) ;
#5413 = DIRECTION ( 'NONE',  ( 0.000000000000000000, -0.9510565162951502005, -0.3090169943749581649 ) ) ;
#5414 = CARTESIAN_POINT ( 'NONE',  ( -90.00000000009001155, -38.00000000000000000, -40.00000000000000000 ) ) ;
#5415 = EDGE_LOOP ( 'NONE', ( #13884, #8621, #11743, #1512 ) ) ;
#5416 = CARTESIAN_POINT ( 'NONE',  ( -8.060728450267886203, -24.77235419320996002, -2.000000000000000000 ) ) ;
#5418 = VERTEX_POINT ( 'NONE', #4648 ) ;
#5417 = ADVANCED_FACE ( 'NONE', ( #1976 ), #6080, .F. ) ;
#5419 = EDGE_CURVE ( 'NONE', #4075, #13818, #2659, .T. ) ;
#5420 = DIRECTION ( 'NONE',  ( -1.000000000000000000, -0.000000000000000000, -0.000000000000000000 ) ) ;
#5421 = ADVANCED_FACE ( 'NONE', ( #17982 ), #8738, .T. ) ;
#5422 = PLANE ( 'NONE',  #6161 ) ;
#5423 = ORIENTED_EDGE ( 'NONE', *, *, #14064, .F. ) ;
#5424 = ORIENTED_EDGE ( 'NONE', *, *, #8900, .T. ) ;
#5425 = PRESENTATION_STYLE_ASSIGNMENT (( #18274 ) ) ;
#5426 =( LENGTH_UNIT ( ) NAMED_UNIT ( * ) SI_UNIT ( .MILLI., .METRE. ) );
#5427 = VERTEX_POINT ( 'NONE', #6170 ) ;
#5428 = CARTESIAN_POINT ( 'NONE',  ( 0.000000000000000000, 11.24999999999999645, 0.000000000000000000 ) ) ;
#5429 = DIRECTION ( 'NONE',  ( 0.000000000000000000, 0.000000000000000000, 1.000000000000000000 ) ) ;
#5430 = CIRCLE ( 'NONE', #7845, 5.384454397937118664 ) ;
#5431 = EDGE_CURVE ( 'NONE', #4385, #17139, #18161, .T. ) ;
#5432 = VECTOR ( 'NONE', #3540, 1000.000000000000000 ) ;
#5433 = AXIS2_PLACEMENT_3D ( 'NONE', #9473, #821, #921 ) ;
#5434 = CIRCLE ( 'NONE', #16368, 10.00000000000000888 ) ;
#5435 = VERTEX_POINT ( 'NONE', #16374 ) ;
#5436 = AXIS2_PLACEMENT_3D ( 'NONE', #16796, #6414, #8128 ) ;
#5437 = ORIENTED_EDGE ( 'NONE', *, *, #8880, .T. ) ;
#5438 = DIRECTION ( 'NONE',  ( 1.000000000000000000, 0.000000000000000000, 0.000000000000000000 ) ) ;
#5439 = CYLINDRICAL_SURFACE ( 'NONE', #15661, 63.00000000006298961 ) ;
#5440 = LINE ( 'NONE', #18665, #16339 ) ;
#5441 = DIRECTION ( 'NONE',  ( -1.000000000000000000, -0.000000000000000000, -0.000000000000000000 ) ) ;
#5442 = AXIS2_PLACEMENT_3D ( 'NONE', #3518, #10745, #16477 ) ;
#5443 = DIRECTION ( 'NONE',  ( 1.000000000000000000, 0.000000000000000000, -0.000000000000000000 ) ) ;
#5444 = CARTESIAN_POINT ( 'NONE',  ( 0.000000000000000000, -23.88582760061464683, -22.76987570971553865 ) ) ;
#5445=STYLED_ITEM('',(#18890),#15813);
#5446 = CYLINDRICAL_SURFACE ( 'NONE', #3530, 2.649999999999995914 ) ;
#5447 = ORIENTED_EDGE ( 'NONE', *, *, #4957, .F. ) ;
#5448 = AXIS2_PLACEMENT_3D ( 'NONE', #2550, #18173, #6550 ) ;
#5449 = FACE_OUTER_BOUND ( 'NONE', #13440, .T. ) ;
#5450 = CARTESIAN_POINT ( 'NONE',  ( -10.00000000000000000, 0.000000000000000000, 0.000000000000000000 ) ) ;
#5451 = FACE_OUTER_BOUND ( 'NONE', #6798, .T. ) ;
#5452 = LINE ( 'NONE', #11253, #3736 ) ;
#5453 = ADVANCED_FACE ( 'NONE', ( #14942 ), #1883, .T. ) ;
#5454 = ORIENTED_EDGE ( 'NONE', *, *, #10484, .F. ) ;
#5455 = AXIS2_PLACEMENT_3D ( 'NONE', #4677, #124, #3159 ) ;
#5456 = CIRCLE ( 'NONE', #16092, 25.00000000000000000 ) ;
#5457 = EDGE_LOOP ( 'NONE', ( #5343, #5797, #4237, #13548 ) ) ;
#5458 = AXIS2_PLACEMENT_3D ( 'NONE', #7109, #12933, #17136 ) ;
#5459 = ORIENTED_EDGE ( 'NONE', *, *, #15873, .T. ) ;
#5460 = LINE ( 'NONE', #11259, #17243 ) ;
#5461 = DIRECTION ( 'NONE',  ( -1.000000000000000000, 0.000000000000000000, 0.000000000000000000 ) ) ;
#5462 = DIRECTION ( 'NONE',  ( 0.000000000000000000, 0.000000000000000000, -1.000000000000000000 ) ) ;
#5463 = DIRECTION ( 'NONE',  ( 1.000000000000000000, -0.000000000000000000, -0.000000000000000000 ) ) ;
#5464 = EDGE_CURVE ( 'NONE', #7978, #6225, #10572, .T. ) ;
#5465 = CARTESIAN_POINT ( 'NONE',  ( 10.04305231718605285, -30.00000000000000000, -30.90933677959240811 ) ) ;
#5466 = AXIS2_PLACEMENT_3D ( 'NONE', #15441, #16779, #8104 ) ;
#5467 = CARTESIAN_POINT ( 'NONE',  ( 11.14999999999999680, 3.067740231864120904E-15, -25.00000000000000711 ) ) ;
#5468 = CARTESIAN_POINT ( 'NONE',  ( -117.1020693116508085, -38.00000000000000000, 19.69080595179778115 ) ) ;
#5469 = ORIENTED_EDGE ( 'NONE', *, *, #16754, .T. ) ;
#5470 = DIRECTION ( 'NONE',  ( -1.000000000000000000, 0.000000000000000000, 0.000000000000000000 ) ) ;
#5471 = ORIENTED_EDGE ( 'NONE', *, *, #16766, .F. ) ;
#5472 = AXIS2_PLACEMENT_3D ( 'NONE', #13696, #1966, #18155 ) ;
#5473 = ADVANCED_FACE ( 'NONE', ( #5509 ), #12644, .T. ) ;
#5474 = DIRECTION ( 'NONE',  ( 0.000000000000000000, 1.000000000000000000, 0.000000000000000000 ) ) ;
#5475 = DIRECTION ( 'NONE',  ( 0.000000000000000000, 0.8910065241883654563, 0.4539904997395512454 ) ) ;
#5476 = VERTEX_POINT ( 'NONE', #18453 ) ;
#5477 = DIRECTION ( 'NONE',  ( 0.000000000000000000, 0.000000000000000000, -1.000000000000000000 ) ) ;
#5478 = DIRECTION ( 'NONE',  ( 6.123233995736766036E-17, -1.000000000000000000, 0.000000000000000000 ) ) ;
#5479 = CARTESIAN_POINT ( 'NONE',  ( 10.00000000000000000, 15.68049343255996320, 29.03656532225568654 ) ) ;
#5480 = VERTEX_POINT ( 'NONE', #5414 ) ;
#5481 = AXIS2_PLACEMENT_3D ( 'NONE', #1702, #6088, #371 ) ;
#5482 = AXIS2_PLACEMENT_3D ( 'NONE', #6517, #15104, #16618 ) ;
#5483 = DIRECTION ( 'NONE',  ( -1.000000000000000000, -0.000000000000000000, 0.000000000000000000 ) ) ;
#5484 = CARTESIAN_POINT ( 'NONE',  ( 4.211140560182196957, -2.431303136016555122, -3.745885042887436622 ) ) ;
#5485 = DIRECTION ( 'NONE',  ( 0.000000000000000000, -1.000000000000000000, 0.000000000000000000 ) ) ;
#5486 = EDGE_CURVE ( 'NONE', #6276, #2833, #16967, .T. ) ;
#5487 = DIRECTION ( 'NONE',  ( -0.000000000000000000, -0.000000000000000000, -1.000000000000000000 ) ) ;
#5488 = DIRECTION ( 'NONE',  ( -0.000000000000000000, -1.000000000000000000, -0.000000000000000000 ) ) ;
#5489 = ORIENTED_EDGE ( 'NONE', *, *, #16912, .T. ) ;
#5490 = DIRECTION ( 'NONE',  ( -1.000000000000000000, 0.000000000000000000, -0.000000000000000000 ) ) ;
#5491 = DIRECTION ( 'NONE',  ( -1.000000000000000000, -0.000000000000000000, -0.000000000000000000 ) ) ;
#5492 = CARTESIAN_POINT ( 'NONE',  ( 10.00000000000000000, 0.000000000000000000, 0.000000000000000000 ) ) ;
#5493 = EDGE_LOOP ( 'NONE', ( #11221, #4105, #13045, #12475, #7588, #12766, #18255, #10439, #5993, #5677, #4587, #4546, #8896, #16981, #8446, #6815 ) ) ;
#5494 = ORIENTED_EDGE ( 'NONE', *, *, #7706, .T. ) ;
#5495 = CARTESIAN_POINT ( 'NONE',  ( 45.00000000000000000, 0.000000000000000000, -2.650000000000511946 ) ) ;
#5496 = PRESENTATION_LAYER_ASSIGNMENT (  '', '', ( #622 ) ) ;
#5497 = ORIENTED_EDGE ( 'NONE', *, *, #11461, .F. ) ;
#5498 = DIRECTION ( 'NONE',  ( -1.000000000000000000, 0.000000000000000000, -0.000000000000000000 ) ) ;
#5499 = EDGE_CURVE ( 'NONE', #11085, #3960, #6652, .T. ) ;
#5500 = DIRECTION ( 'NONE',  ( -1.000000000000000000, 0.000000000000000000, 0.000000000000000000 ) ) ;
#5501 = ADVANCED_FACE ( 'NONE', ( #2456 ), #11179, .F. ) ;
#5502 = FACE_OUTER_BOUND ( 'NONE', #11906, .T. ) ;
#5503 = ORIENTED_EDGE ( 'NONE', *, *, #7484, .T. ) ;
#5505 = LINE ( 'NONE', #15686, #17075 ) ;
#5504 = AXIS2_PLACEMENT_3D ( 'NONE', #4353, #8454, #11393 ) ;
#5506 = EDGE_LOOP ( 'NONE', ( #859, #1211, #18336, #17947 ) ) ;
#5507 = CARTESIAN_POINT ( 'NONE',  ( 10.00000000000000000, 0.000000000000000000, 0.000000000000000000 ) ) ;
#5508 = FACE_OUTER_BOUND ( 'NONE', #16654, .T. ) ;
#5509 = FACE_OUTER_BOUND ( 'NONE', #9503, .T. ) ;
#5510 = ORIENTED_EDGE ( 'NONE', *, *, #9189, .F. ) ;
#5511 = PLANE ( 'NONE',  #13605 ) ;
#5512 = VERTEX_POINT ( 'NONE', #947 ) ;
#5513 = DIRECTION ( 'NONE',  ( -1.000000000000000000, -0.000000000000000000, -0.000000000000000000 ) ) ;
#5514 = CARTESIAN_POINT ( 'NONE',  ( -9.345251662538453630, -28.92794965710190525, -2.000000000000000000 ) ) ;
#5515 = VERTEX_POINT ( 'NONE', #16938 ) ;
#5516 = ORIENTED_EDGE ( 'NONE', *, *, #5431, .F. ) ;
#5517 = DIRECTION ( 'NONE',  ( 0.000000000000000000, 0.8090169943749487835, -0.5877852522924713607 ) ) ;
#5518 =( NAMED_UNIT ( * ) SI_UNIT ( $, .STERADIAN. ) SOLID_ANGLE_UNIT ( ) );
#5520 = EDGE_CURVE ( 'NONE', #6939, #12056, #13788, .T. ) ;
#5519 = ORIENTED_EDGE ( 'NONE', *, *, #12027, .F. ) ;
#5521 = CARTESIAN_POINT ( 'NONE',  ( 0.000000000000000000, -57.83923611457337444, 24.97244012287480430 ) ) ;
#5522 = CARTESIAN_POINT ( 'NONE',  ( -2.000000000000000000, -6.429618962271402616, 0.000000000000000000 ) ) ;
#5523 = AXIS2_PLACEMENT_3D ( 'NONE', #8339, #18707, #4329 ) ;
#5524 = ADVANCED_FACE ( 'NONE', ( #16842 ), #1160, .T. ) ;
#5525 = EDGE_CURVE ( 'NONE', #13562, #13630, #8149, .T. ) ;
#5526 = CIRCLE ( 'NONE', #12542, 24.00000000002399858 ) ;
#5527 = ORIENTED_EDGE ( 'NONE', *, *, #13557, .F. ) ;
#5528 = ADVANCED_FACE ( 'NONE', ( #12460 ), #1131, .T. ) ;
#5529 = VERTEX_POINT ( 'NONE', #15227 ) ;
#5530 = DIRECTION ( 'NONE',  ( 0.000000000000000000, 0.000000000000000000, 1.000000000000000000 ) ) ;
#5531 = DIRECTION ( 'NONE',  ( -1.000000000000000000, -0.000000000000000000, -0.000000000000000000 ) ) ;
#5533 = EDGE_CURVE ( 'NONE', #13213, #11810, #9968, .T. ) ;
#5532 = PLANE ( 'NONE',  #17841 ) ;
#5534 = FACE_BOUND ( 'NONE', #1516, .T. ) ;
#5535 = CIRCLE ( 'NONE', #1245, 2.649999999999985700 ) ;
#5536 = DIRECTION ( 'NONE',  ( 0.000000000000000000, 0.5877852522924685852, 0.8090169943749507819 ) ) ;
#5537 = LINE ( 'NONE', #8483, #16804 ) ;
#5538 = FACE_OUTER_BOUND ( 'NONE', #8958, .T. ) ;
#5539 = ORIENTED_EDGE ( 'NONE', *, *, #3757, .T. ) ;
#5540 = CARTESIAN_POINT ( 'NONE',  ( 0.000000000000000000, 11.24999999999999467, 0.000000000000000000 ) ) ;
#5541 = CARTESIAN_POINT ( 'NONE',  ( 10.00000000000000000, -4.381479206523214209, 32.70783759231085241 ) ) ;
#5542 = ADVANCED_FACE ( 'NONE', ( #12549 ), #7822, .T. ) ;
#5543 = AXIS2_PLACEMENT_3D ( 'NONE', #14403, #1362, #15926 ) ;
#5544 = CARTESIAN_POINT ( 'NONE',  ( 0.000000000000000000, 0.000000000000000000, 0.000000000000000000 ) ) ;
#5545 = ORIENTED_EDGE ( 'NONE', *, *, #1094, .T. ) ;
#5546 = ORIENTED_EDGE ( 'NONE', *, *, #18702, .T. ) ;
#5547 = EDGE_CURVE ( 'NONE', #7753, #18363, #10267, .T. ) ;
#5548 = ORIENTED_EDGE ( 'NONE', *, *, #8671, .F. ) ;
#5550 = DIRECTION ( 'NONE',  ( 0.000000000000000000, -0.9510565162951502005, -0.3090169943749579984 ) ) ;
#5549 = AXIS2_PLACEMENT_3D ( 'NONE', #3922, #7132, #15534 ) ;
#5551 = CARTESIAN_POINT ( 'NONE',  ( 10.00000000000000000, 56.37237871411035428, -1.017308535511785683 ) ) ;
#5552 = ORIENTED_EDGE ( 'NONE', *, *, #10587, .F. ) ;
#5553 = EDGE_CURVE ( 'NONE', #16785, #15687, #6325, .T. ) ;
#5554 = CARTESIAN_POINT ( 'NONE',  ( 0.000000000000000000, 9.514709542736897063, 24.46385708179987262 ) ) ;
#5555 = CARTESIAN_POINT ( 'NONE',  ( -36.40576474687271258, 10.00000000000000000, -26.45033635316118747 ) ) ;
#5556 = DIRECTION ( 'NONE',  ( -1.000000000000000000, -0.000000000000000000, 0.000000000000000000 ) ) ;
#5557 = DIRECTION ( 'NONE',  ( 1.000000000000000000, -0.000000000000000000, -0.000000000000000000 ) ) ;
#5558 = VERTEX_POINT ( 'NONE', #8176 ) ;
#5559 = CARTESIAN_POINT ( 'NONE',  ( 0.000000000000000000, 40.19788616105680035, -48.50907078259338334 ) ) ;
#5560 = VERTEX_POINT ( 'NONE', #3892 ) ;
#5561 = PRODUCT_DEFINITION_SHAPE ( 'NONE', 'NONE',  #18184 ) ;
#5562 = PLANE ( 'NONE',  #5890 ) ;
#5563 = DIRECTION ( 'NONE',  ( 0.000000000000000000, 0.000000000000000000, 1.000000000000000000 ) ) ;
#5564 = EDGE_LOOP ( 'NONE', ( #11897, #15488, #11051, #4310 ) ) ;
#5565 = CARTESIAN_POINT ( 'NONE',  ( 0.000000000000000000, 0.000000000000000000, 0.000000000000000000 ) ) ;
#5566 = CARTESIAN_POINT ( 'NONE',  ( -117.1020693116507942, -43.00000000000000000, 19.69080595179777760 ) ) ;
#5567 = DIRECTION ( 'NONE',  ( -1.000000000000000000, 0.000000000000000000, -0.000000000000000000 ) ) ;
#5568 = ORIENTED_EDGE ( 'NONE', *, *, #8841, .T. ) ;
#5569 = CARTESIAN_POINT ( 'NONE',  ( 5.000000000000000000, 53.22058882792197210, 33.71303790549294632 ) ) ;
#5570 = CARTESIAN_POINT ( 'NONE',  ( 5.200000000000002842, 0.000000000000000000, -2.700000000000000622 ) ) ;
#5571 = CARTESIAN_POINT ( 'NONE',  ( 0.000000000000000000, 40.58063702438398224, -39.14194549634321163 ) ) ;
#5572 = EDGE_CURVE ( 'NONE', #12788, #280, #12747, .T. ) ;
#5573 = CARTESIAN_POINT ( 'NONE',  ( 0.000000000000000000, -40.19788616105644508, 48.50907078259368177 ) ) ;
#5574 = AXIS2_PLACEMENT_3D ( 'NONE', #16824, #16734, #9568 ) ;
#5575 = CIRCLE ( 'NONE', #3439, 25.00000000000000355 ) ;
#5576 = DIRECTION ( 'NONE',  ( 0.000000000000000000, 0.3090169943749481174, -0.9510565162951533091 ) ) ;
#5577 = EDGE_LOOP ( 'NONE', ( #14488, #15831, #12360, #16395 ) ) ;
#5578 = DIRECTION ( 'NONE',  ( 0.000000000000000000, 1.000000000000000000, 0.000000000000000000 ) ) ;
#5579 = CARTESIAN_POINT ( 'NONE',  ( 10.00000000000000000, -23.88582760061497368, 22.76987570971519048 ) ) ;
#5580 = CARTESIAN_POINT ( 'NONE',  ( -56.50000000009000445, -30.00000000000000000, 2.650000000000374278 ) ) ;
#5581 = ORIENTED_EDGE ( 'NONE', *, *, #2590, .F. ) ;
#5582 = ORIENTED_EDGE ( 'NONE', *, *, #17398, .T. ) ;
#5583 = FACE_OUTER_BOUND ( 'NONE', #14821, .T. ) ;
#5584 = ORIENTED_EDGE ( 'NONE', *, *, #14665, .T. ) ;
#5585 = CYLINDRICAL_SURFACE ( 'NONE', #11238, 56.24900000005625600 ) ;
#5586 = EDGE_CURVE ( 'NONE', #16250, #14912, #9345, .T. ) ;
#5587 = CIRCLE ( 'NONE', #1037, 24.00000000002399858 ) ;
#5588 = EDGE_CURVE ( 'NONE', #3333, #3720, #3907, .T. ) ;
#5589 = DIRECTION ( 'NONE',  ( -1.000000000000000000, 0.000000000000000000, 0.000000000000000000 ) ) ;
#5590 = CARTESIAN_POINT ( 'NONE',  ( 10.00000000000000000, 0.000000000000000000, 0.000000000000000000 ) ) ;
#5591 = ORIENTED_EDGE ( 'NONE', *, *, #18543, .T. ) ;
#5592 = DIRECTION ( 'NONE',  ( -1.000000000000000000, -0.000000000000000000, -0.000000000000000000 ) ) ;
#5593 = EDGE_LOOP ( 'NONE', ( #5669, #6351, #10190, #1540 ) ) ;
#5595 = CARTESIAN_POINT ( 'NONE',  ( 0.000000000000000000, 25.42247726998032320, -12.18267823974723640 ) ) ;
#5594 = UNCERTAINTY_MEASURE_WITH_UNIT (LENGTH_MEASURE( 1.000000000000000082E-05 ), #8899, 'distance_accuracy_value', 'NONE');
#5596 = DIRECTION ( 'NONE',  ( 0.000000000000000000, 1.000000000000000000, 0.000000000000000000 ) ) ;
#5597 = ORIENTED_EDGE ( 'NONE', *, *, #12616, .F. ) ;
#5598 = CARTESIAN_POINT ( 'NONE',  ( 10.00000000000000000, 0.000000000000000000, 0.000000000000000000 ) ) ;
#5599 = ORIENTED_EDGE ( 'NONE', *, *, #10061, .F. ) ;
#5600 = CARTESIAN_POINT ( 'NONE',  ( 10.00000000000000000, -32.31183295104739273, -46.20417134726167063 ) ) ;
#5601 = FACE_BOUND ( 'NONE', #6065, .T. ) ;
#5602 = ORIENTED_EDGE ( 'NONE', *, *, #8999, .T. ) ;
#5603 = ORIENTED_EDGE ( 'NONE', *, *, #4945, .F. ) ;
#5604 = CARTESIAN_POINT ( 'NONE',  ( -2.499999999999999556, 3.061616997868382648E-16, 3.469446951953614189E-15 ) ) ;
#5605 = ORIENTED_EDGE ( 'NONE', *, *, #9706, .F. ) ;
#5606 = CYLINDRICAL_SURFACE ( 'NONE', #12128, 56.24900000005625600 ) ;
#5607 = DIRECTION ( 'NONE',  ( -1.000000000000000000, 0.000000000000000000, -0.000000000000000000 ) ) ;
#5608 = STYLED_ITEM ( 'NONE', ( #12339 ), #4227 ) ;
#5609 = CARTESIAN_POINT ( 'NONE',  ( 130.0000000000000000, -34.99999999999999289, 125.0000000000000000 ) ) ;
#5610 = ORIENTED_EDGE ( 'NONE', *, *, #4241, .T. ) ;
#5611 = ORIENTED_EDGE ( 'NONE', *, *, #18422, .T. ) ;
#5612 = DIRECTION ( 'NONE',  ( -1.000000000000000000, -0.000000000000000000, 0.000000000000000000 ) ) ;
#5613 = CARTESIAN_POINT ( 'NONE',  ( 10.00000000000000000, -16.60877409751153522, -20.32630374611203194 ) ) ;
#5614 = FACE_OUTER_BOUND ( 'NONE', #8466, .T. ) ;
#5615 = DIRECTION ( 'NONE',  ( -1.000000000000000000, -0.000000000000000000, -0.000000000000000000 ) ) ;
#5616 = DIRECTION ( 'NONE',  ( 0.000000000000000000, 0.9510565162951543083, -0.3090169943749447312 ) ) ;
#5617 = DIRECTION ( 'NONE',  ( -1.000000000000000000, -0.000000000000000000, -0.000000000000000000 ) ) ;
#5618 = DIRECTION ( 'NONE',  ( 1.000000000000000000, 0.000000000000000000, 0.000000000000000000 ) ) ;
#5619 = ORIENTED_EDGE ( 'NONE', *, *, #11326, .T. ) ;
#5620 = DIRECTION ( 'NONE',  ( 0.000000000000000000, 0.000000000000000000, -1.000000000000000000 ) ) ;
#5621 = ADVANCED_FACE ( 'NONE', ( #9589 ), #15409, .T. ) ;
#5622 = EDGE_CURVE ( 'NONE', #3664, #2762, #9047, .T. ) ;
#5623 = CARTESIAN_POINT ( 'NONE',  ( 10.00000000000000000, 0.000000000000000000, 56.24900000005625600 ) ) ;
#5624 = AXIS2_PLACEMENT_3D ( 'NONE', #3476, #10614, #4983 ) ;
#5625 = ADVANCED_FACE ( 'NONE', ( #159 ), #18730, .T. ) ;
#5626 = DIRECTION ( 'NONE',  ( 1.000000000000000000, 0.000000000000000000, 0.000000000000000000 ) ) ;
#5627 = DIRECTION ( 'NONE',  ( 0.000000000000000000, 0.000000000000000000, 1.000000000000000000 ) ) ;
#5628 = CIRCLE ( 'NONE', #11397, 24.00000000002399858 ) ;
#5629 = EDGE_CURVE ( 'NONE', #1871, #435, #7233, .T. ) ;
#5630 = VERTEX_POINT ( 'NONE', #5956 ) ;
#5631 = EDGE_CURVE ( 'NONE', #17331, #9794, #7105, .T. ) ;
#5632 = ORIENTED_EDGE ( 'NONE', *, *, #18805, .T. ) ;
#5633 = AXIS2_PLACEMENT_3D ( 'NONE', #9061, #1828, #13454 ) ;
#5634 = FACE_OUTER_BOUND ( 'NONE', #3596, .T. ) ;
#5635 = LINE ( 'NONE', #15639, #6094 ) ;
#5636 = ADVANCED_FACE ( 'NONE', ( #4355 ), #8821, .F. ) ;
#5637 = CIRCLE ( 'NONE', #16281, 2.649999999999995914 ) ;
#5638 = VERTEX_POINT ( 'NONE', #8459 ) ;
#5639 = DIRECTION ( 'NONE',  ( -1.000000000000000000, 0.000000000000000000, 0.000000000000000000 ) ) ;
#5640 = VECTOR ( 'NONE', #17840, 1000.000000000000000 ) ;
#5641 = CARTESIAN_POINT ( 'NONE',  ( 0.000000000000000000, -26.49895292617967257, -49.76630880786338196 ) ) ;
#5642 = DIRECTION ( 'NONE',  ( 0.000000000000000000, 0.000000000000000000, 1.000000000000000000 ) ) ;
#5643 = DIRECTION ( 'NONE',  ( 0.000000000000000000, 0.000000000000000000, 1.000000000000000000 ) ) ;
#5644 = CARTESIAN_POINT ( 'NONE',  ( 0.000000000000000000, -1.178949249685213863, 2.042000000000001148 ) ) ;
#5645 = ORIENTED_EDGE ( 'NONE', *, *, #4002, .T. ) ;
#5646 = FACE_OUTER_BOUND ( 'NONE', #6443, .T. ) ;
#5647 = ORIENTED_EDGE ( 'NONE', *, *, #7749, .T. ) ;
#5648 = ADVANCED_FACE ( 'NONE', ( #11779 ), #14275, .T. ) ;
#5649 = SURFACE_STYLE_FILL_AREA ( #15844 ) ;
#5650 = DIRECTION ( 'NONE',  ( 0.000000000000000000, 0.000000000000000000, 1.000000000000000000 ) ) ;
#5651 = ORIENTED_EDGE ( 'NONE', *, *, #11346, .T. ) ;
#5652 = CIRCLE ( 'NONE', #3216, 2.649999999999999467 ) ;
#5653 = ITEM_DEFINED_TRANSFORMATION ( 'NONE', 'NONE', #6525,  #8017 ) ;
#5654 = LINE ( 'NONE', #2707, #2654 ) ;
#5655 = ORIENTED_EDGE ( 'NONE', *, *, #2483, .F. ) ;
#5656 = AXIS2_PLACEMENT_3D ( 'NONE', #17124, #9869, #2164 ) ;
#5657 = VECTOR ( 'NONE', #3074, 1000.000000000000000 ) ;
#5658 = EDGE_CURVE ( 'NONE', #9105, #10779, #3588, .T. ) ;
#5659 = FACE_BOUND ( 'NONE', #2580, .T. ) ;
#5660 = CARTESIAN_POINT ( 'NONE',  ( 4.207491450040567571, -2.029819825146485179, -3.671670828759567407 ) ) ;
#5661 = CIRCLE ( 'NONE', #17802, 56.24900000005625600 ) ;
#5662 = VECTOR ( 'NONE', #2039, 1000.000000000000000 ) ;
#5663 = DIRECTION ( 'NONE',  ( 0.000000000000000000, 0.000000000000000000, 1.000000000000000000 ) ) ;
#5664 = LINE ( 'NONE', #7003, #7950 ) ;
#5665 = AXIS2_PLACEMENT_3D ( 'NONE', #18393, #1272, #12792 ) ;
#5666 = AXIS2_PLACEMENT_3D ( 'NONE', #4326, #15940, #9852 ) ;
#5667 = CARTESIAN_POINT ( 'NONE',  ( 10.00000000000000000, 38.81885513159988932, 40.70683587897971734 ) ) ;
#5668 = VECTOR ( 'NONE', #286, 1000.000000000000000 ) ;
#5669 = ORIENTED_EDGE ( 'NONE', *, *, #880, .T. ) ;
#5670 = SHAPE_REPRESENTATION ( 'spur gear 1_iso_ISO - Spur gear 3M 40T 20PA 10FW ---S40A75H50L60.0N', ( #8017 ), #2559 ) ;
#5671 = CARTESIAN_POINT ( 'NONE',  ( 10.00000000000000000, 7.478235706489787304, -55.74967257055874370 ) ) ;
#5672 = DIRECTION ( 'NONE',  ( 0.000000000000000000, 0.000000000000000000, -1.000000000000000000 ) ) ;
#5673 = FACE_OUTER_BOUND ( 'NONE', #15678, .T. ) ;
#5674 = ORIENTED_EDGE ( 'NONE', *, *, #16442, .F. ) ;
#5675 = VERTEX_POINT ( 'NONE', #7392 ) ;
#5676 = DIRECTION ( 'NONE',  ( 0.000000000000000000, 0.000000000000000000, 1.000000000000000000 ) ) ;
#5677 = ORIENTED_EDGE ( 'NONE', *, *, #14024, .T. ) ;
#5678 = AXIS2_PLACEMENT_3D ( 'NONE', #17005, #3957, #5180 ) ;
#5679 = VECTOR ( 'NONE', #13620, 1000.000000000000000 ) ;
#5680 = EDGE_CURVE ( 'NONE', #10144, #18793, #16664, .T. ) ;
#5681 = CIRCLE ( 'NONE', #9629, 10.00000000000000888 ) ;
#5682 = AXIS2_PLACEMENT_3D ( 'NONE', #1070, #15736, #8401 ) ;
#5683 = CIRCLE ( 'NONE', #7803, 26.24900000002625333 ) ;
#5684 = CARTESIAN_POINT ( 'NONE',  ( -10.00000000000000000, -5.117658387065794099E-13, -47.64999999999999858 ) ) ;
#5685 = CARTESIAN_POINT ( 'NONE',  ( 0.000000000000000000, 1.305124410222461284, -2.000000000000000000 ) ) ;
#5686 = VERTEX_POINT ( 'NONE', #1315 ) ;
#5687 = DIRECTION ( 'NONE',  ( -0.9967691390334607604, -0.000000000000000000, 0.08031988216184954288 ) ) ;
#5688 = AXIS2_PLACEMENT_3D ( 'NONE', #5322, #11132, #16960 ) ;
#5689 = EDGE_LOOP ( 'NONE', ( #8808, #5364, #1673, #15411 ) ) ;
#5691 = AXIS2_PLACEMENT_3D ( 'NONE', #14445, #13035, #8830 ) ;
#5690 = DIRECTION ( 'NONE',  ( 1.000000000000000000, 0.000000000000000000, 0.000000000000000000 ) ) ;
#5692 = EDGE_LOOP ( 'NONE', ( #14446, #6636, #16443 ) ) ;
#5693 = CARTESIAN_POINT ( 'NONE',  ( -3.999999999999999112, 1.539600717838996324, -3.300726591567078039 ) ) ;
#5694 = VERTEX_POINT ( 'NONE', #15690 ) ;
#5695 = CIRCLE ( 'NONE', #11148, 33.00000000003299760 ) ;
#5696 = EDGE_CURVE ( 'NONE', #17469, #17641, #8450, .T. ) ;
#5697 = LINE ( 'NONE', #2835, #8059 ) ;
#5698 = CARTESIAN_POINT ( 'NONE',  ( 2.500000000000000000, -2.629050547790028551E-15, -2.041999999999999815 ) ) ;
#5699 = CIRCLE ( 'NONE', #17551, 33.00000000003299760 ) ;
#5700 = ORIENTED_EDGE ( 'NONE', *, *, #8890, .F. ) ;
#5701 = ORIENTED_EDGE ( 'NONE', *, *, #705, .T. ) ;
#5702 = CIRCLE ( 'NONE', #10860, 24.00000000002400213 ) ;
#5703 = DIRECTION ( 'NONE',  ( 0.000000000000000000, 0.000000000000000000, 1.000000000000000000 ) ) ;
#5704 = ADVANCED_FACE ( 'NONE', ( #77 ), #1228, .T. ) ;
#5705 = FILL_AREA_STYLE_COLOUR ( '', #8645 ) ;
#5706 = EDGE_LOOP ( 'NONE', ( #8634, #340 ) ) ;
#5707 = DIRECTION ( 'NONE',  ( 1.000000000000000000, -0.000000000000000000, 0.000000000000000000 ) ) ;
#5708 = CIRCLE ( 'NONE', #3879, 56.24900000005627021 ) ;
#5709 = LINE ( 'NONE', #8646, #15877 ) ;
#5710 = CIRCLE ( 'NONE', #12090, 56.24900000005625600 ) ;
#5711 = VECTOR ( 'NONE', #5642, 1000.000000000000000 ) ;
#5712 = ORIENTED_EDGE ( 'NONE', *, *, #3120, .F. ) ;
#5713 = VERTEX_POINT ( 'NONE', #11600 ) ;
#5714 = DIRECTION ( 'NONE',  ( 0.000000000000000000, 1.000000000000000000, 0.000000000000000000 ) ) ;
#5715 = CARTESIAN_POINT ( 'NONE',  ( 5.200000000000002842, 3.061616997868383634E-16, -2.500000000000000444 ) ) ;
#5716 = CARTESIAN_POINT ( 'NONE',  ( 0.000000000000000000, -5.940243314903989713, -32.46095361140699254 ) ) ;
#5717 = CARTESIAN_POINT ( 'NONE',  ( -4.000000000000000000, 1.700094919196744270, -3.320312364301766017 ) ) ;
#5718 = DIRECTION ( 'NONE',  ( -1.000000000000000000, 0.000000000000000000, 0.000000000000000000 ) ) ;
#5719 = DIRECTION ( 'NONE',  ( 0.000000000000000000, 0.000000000000000000, 1.000000000000000000 ) ) ;
#5720 = AXIS2_PLACEMENT_3D ( 'NONE', #7304, #5874, #11685 ) ;
#5721 = CARTESIAN_POINT ( 'NONE',  ( -4.078421086530219064, -3.990950201428956845, -1.000000000000000000 ) ) ;
#5722 = VERTEX_POINT ( 'NONE', #12841 ) ;
#5723 = CARTESIAN_POINT ( 'NONE',  ( 0.000000000000000000, 11.24999999999999645, 0.000000000000000000 ) ) ;
#5724 = PRESENTATION_STYLE_ASSIGNMENT (( #8575 ) ) ;
#5725 = AXIS2_PLACEMENT_3D ( 'NONE', #911, #15469, #11065 ) ;
#5726 = ORIENTED_EDGE ( 'NONE', *, *, #11988, .T. ) ;
#5727 = CARTESIAN_POINT ( 'NONE',  ( 10.00000000000000000, 0.000000000000000000, 0.000000000000000000 ) ) ;
#5728 = DIRECTION ( 'NONE',  ( 0.000000000000000000, 0.000000000000000000, -1.000000000000000000 ) ) ;
#5729 = CIRCLE ( 'NONE', #12952, 2.649999999999985700 ) ;
#5730 = AXIS2_PLACEMENT_3D ( 'NONE', #2477, #9431, #14006 ) ;
#5731 = EDGE_LOOP ( 'NONE', ( #12461, #6385, #874, #10336 ) ) ;
#5732 = CIRCLE ( 'NONE', #12415, 40.00000000000000000 ) ;
#5733 = ADVANCED_FACE ( 'NONE', ( #10158, #4271, #10071, #17218, #1398, #15964, #8631 ), #4174, .T. ) ;
#5734 = ORIENTED_EDGE ( 'NONE', *, *, #4987, .F. ) ;
#5735 = CARTESIAN_POINT ( 'NONE',  ( 2.449293598294706513E-15, -34.99999999999999289, -20.00000000000000000 ) ) ;
#5736 = EDGE_CURVE ( 'NONE', #17978, #1435, #2919, .T. ) ;
#5737 = DIRECTION ( 'NONE',  ( 0.000000000000000000, 0.000000000000000000, 1.000000000000000000 ) ) ;
#5738 = CIRCLE ( 'NONE', #12113, 56.24900000005624889 ) ;
#5739 = VERTEX_POINT ( 'NONE', #1499 ) ;
#5740 = VECTOR ( 'NONE', #4102, 1000.000000000000000 ) ;
#5741 = DIRECTION ( 'NONE',  ( -1.000000000000000000, -0.000000000000000000, 0.000000000000000000 ) ) ;
#5742 = CARTESIAN_POINT ( 'NONE',  ( 0.000000000000000000, -32.31183295104805353, 46.20417134726119457 ) ) ;
#5743 = PRODUCT_RELATED_PRODUCT_CATEGORY ( 'part', '', ( #6337 ) ) ;
#5744 = FACE_OUTER_BOUND ( 'NONE', #8305, .T. ) ;
#5745 = FACE_OUTER_BOUND ( 'NONE', #12586, .T. ) ;
#5746 = CARTESIAN_POINT ( 'NONE',  ( 5.000000000000000000, 58.55669782892493203, -23.24033432160376478 ) ) ;
#5747 = ORIENTED_EDGE ( 'NONE', *, *, #16977, .F. ) ;
#5748 = CARTESIAN_POINT ( 'NONE',  ( -4.144923636027600722, -29.35885059145708098, 0.000000000000000000 ) ) ;
#5749 = ORIENTED_EDGE ( 'NONE', *, *, #15654, .T. ) ;
#5750 = EDGE_CURVE ( 'NONE', #202, #858, #5094, .T. ) ;
#5751 = CARTESIAN_POINT ( 'NONE',  ( 10.00000000000000000, 20.32630374611208879, -16.60877409751146416 ) ) ;
#5752 = CYLINDRICAL_SURFACE ( 'NONE', #8758, 2.396904916527700102 ) ;
#5753 = CIRCLE ( 'NONE', #14262, 5.560781378645573980 ) ;
#5754 = VERTEX_POINT ( 'NONE', #10624 ) ;
#5755 = CIRCLE ( 'NONE', #6662, 0.7500000000000000000 ) ;
#5756 = EDGE_LOOP ( 'NONE', ( #3363, #759, #1729, #4634 ) ) ;
#5757 = ADVANCED_FACE ( 'NONE', ( #13404 ), #6435, .T. ) ;
#5758 = CIRCLE ( 'NONE', #3937, 24.00000000002399858 ) ;
#5759 = VECTOR ( 'NONE', #8985, 1000.000000000000000 ) ;
#5760 = ADVANCED_FACE ( 'NONE', ( #4540 ), #16444, .F. ) ;
#5761 = DIRECTION ( 'NONE',  ( 0.000000000000000000, -0.7071067811865388020, -0.7071067811865562325 ) ) ;
#5762 = EDGE_CURVE ( 'NONE', #13152, #11197, #12398, .T. ) ;
#5763 = CARTESIAN_POINT ( 'NONE',  ( 5.000000000000000000, 5.876895005582427167, 62.72529079327809853 ) ) ;
#5764 = VECTOR ( 'NONE', #8868, 1000.000000000000000 ) ;
#5765 = DIRECTION ( 'NONE',  ( 0.000000000000000000, 0.000000000000000000, 1.000000000000000000 ) ) ;
#5766 = DIRECTION ( 'NONE',  ( 0.000000000000000000, 0.4999999999999990008, -0.8660254037844391517 ) ) ;
#5767 = AXIS2_PLACEMENT_3D ( 'NONE', #10264, #10359, #5798 ) ;
#5768 = EDGE_CURVE ( 'NONE', #9230, #16428, #17896, .T. ) ;
#5769 = CYLINDRICAL_SURFACE ( 'NONE', #12122, 56.24900000005625600 ) ;
#5770 = VERTEX_POINT ( 'NONE', #10434 ) ;
#5771 = EDGE_CURVE ( 'NONE', #9920, #3160, #6948, .T. ) ;
#5772 = DIRECTION ( 'NONE',  ( 1.000000000000000000, 0.000000000000000000, 0.000000000000000000 ) ) ;
#5773 = DIRECTION ( 'NONE',  ( -1.000000000000000000, 0.000000000000000000, 0.000000000000000000 ) ) ;
#5774 = CARTESIAN_POINT ( 'NONE',  ( 10.00000000000000000, -58.55669782892479702, 23.24033432160415913 ) ) ;
#5775 = VERTEX_POINT ( 'NONE', #349 ) ;
#5776 = ORIENTED_EDGE ( 'NONE', *, *, #10124, .F. ) ;
#5777 = CARTESIAN_POINT ( 'NONE',  ( 10.00000000000000000, -24.46385708179990459, 9.514709542736804693 ) ) ;
#5778 = ORIENTED_EDGE ( 'NONE', *, *, #7458, .T. ) ;
#5779 = CIRCLE ( 'NONE', #14893, 24.00000000002399858 ) ;
#5780 = AXIS2_PLACEMENT_3D ( 'NONE', #15587, #10875, #8121 ) ;
#5781 = CARTESIAN_POINT ( 'NONE',  ( 0.000000000000000000, 0.000000000000000000, 26.24900000002624978 ) ) ;
#5782 = CARTESIAN_POINT ( 'NONE',  ( 10.00000000000000000, 27.72801475327282361, 6.913036516934699449 ) ) ;
#5783 = VERTEX_POINT ( 'NONE', #7868 ) ;
#5784 = LINE ( 'NONE', #9782, #636 ) ;
#5785 = CIRCLE ( 'NONE', #10643, 24.00000000002399148 ) ;
#5786 = EDGE_LOOP ( 'NONE', ( #9980, #17221 ) ) ;
#5787 = PRODUCT_DEFINITION_CONTEXT ( 'detailed design', #16821, 'design' ) ;
#5788 = DIRECTION ( 'NONE',  ( 0.000000000000000000, 0.000000000000000000, 1.000000000000000000 ) ) ;
#5789 = ORIENTED_EDGE ( 'NONE', *, *, #16340, .T. ) ;
#5790 = EDGE_CURVE ( 'NONE', #5694, #16829, #11808, .T. ) ;
#5791 = ORIENTED_EDGE ( 'NONE', *, *, #15467, .F. ) ;
#5792 = FACE_OUTER_BOUND ( 'NONE', #18175, .T. ) ;
#5793 = CARTESIAN_POINT ( 'NONE',  ( 10.00000000000000000, -5.940243314904447125, 32.46095361140690727 ) ) ;
#5794 = ORIENTED_EDGE ( 'NONE', *, *, #10503, .T. ) ;
#5795 = VERTEX_POINT ( 'NONE', #3114 ) ;
#5796 = CYLINDRICAL_SURFACE ( 'NONE', #2643, 40.00000000000000000 ) ;
#5797 = ORIENTED_EDGE ( 'NONE', *, *, #13595, .T. ) ;
#5798 = DIRECTION ( 'NONE',  ( 0.000000000000000000, 0.000000000000000000, 1.000000000000000000 ) ) ;
#5799 = AXIS2_PLACEMENT_3D ( 'NONE', #10493, #9073, #14892 ) ;
#5800 = CARTESIAN_POINT ( 'NONE',  ( 0.3865131578947368918, -23.49682122285426189, 0.000000000000000000 ) ) ;
#5801 = VERTEX_POINT ( 'NONE', #17960 ) ;
#5802 = ORIENTED_EDGE ( 'NONE', *, *, #8423, .T. ) ;
#5803 = CARTESIAN_POINT ( 'NONE',  ( 3.309651814758564736, -5.455921364805393026, 0.000000000000000000 ) ) ;
#5804 = FACE_OUTER_BOUND ( 'NONE', #17196, .T. ) ;
#5805 = FACE_OUTER_BOUND ( 'NONE', #8442, .T. ) ;
#5806 = CARTESIAN_POINT ( 'NONE',  ( 10.00000000000000000, 23.24033432160521429, -58.55669782892436359 ) ) ;
#5807 = DIRECTION ( 'NONE',  ( -0.000000000000000000, 1.000000000000000000, -0.000000000000000000 ) ) ;
#5808 = ADVANCED_FACE ( 'NONE', ( #11869 ), #13685, .T. ) ;
#5809 = DIRECTION ( 'NONE',  ( 0.000000000000000000, 0.000000000000000000, -1.000000000000000000 ) ) ;
#5810 = CARTESIAN_POINT ( 'NONE',  ( 0.000000000000000000, -26.50000000000000000, 0.000000000000000000 ) ) ;
#5811 = FACE_BOUND ( 'NONE', #13280, .T. ) ;
#5812 = ORIENTED_EDGE ( 'NONE', *, *, #7619, .T. ) ;
#5813 = PLANE ( 'NONE',  #6063 ) ;
#5814 = VECTOR ( 'NONE', #16934, 1000.000000000000000 ) ;
#5815 = LINE ( 'NONE', #5623, #14495 ) ;
#5816 = ORIENTED_EDGE ( 'NONE', *, *, #1305, .F. ) ;
#5817 = DIRECTION ( 'NONE',  ( -1.000000000000000000, 0.000000000000000000, 0.000000000000000000 ) ) ;
#5818 = DIRECTION ( 'NONE',  ( -1.000000000000000000, -0.000000000000000000, -0.000000000000000000 ) ) ;
#5819 = EDGE_CURVE ( 'NONE', #6455, #1018, #4717, .T. ) ;
#5820 = ORIENTED_EDGE ( 'NONE', *, *, #7851, .T. ) ;
#5821 = AXIS2_PLACEMENT_3D ( 'NONE', #629, #13763, #13586 ) ;
#5822 = EDGE_CURVE ( 'NONE', #5560, #11258, #13588, .T. ) ;
#5823 = CARTESIAN_POINT ( 'NONE',  ( 0.000000000000000000, -27.94286728106390072, -3.730438010304629515 ) ) ;
#5824 = ORIENTED_EDGE ( 'NONE', *, *, #16677, .F. ) ;
#5825 = CARTESIAN_POINT ( 'NONE',  ( 0.1481481481481481122, -4.797713218419819903, -1.000000000000000000 ) ) ;
#5826 = FACE_OUTER_BOUND ( 'NONE', #13608, .T. ) ;
#5827 = VECTOR ( 'NONE', #8470, 1000.000000000000000 ) ;
#5828 = CARTESIAN_POINT ( 'NONE',  ( 34.99999999999999289, 0.000000000000000000, 0.000000000000000000 ) ) ;
#5829 = DIRECTION ( 'NONE',  ( -1.000000000000000000, 0.000000000000000000, 0.000000000000000000 ) ) ;
#5830 = DIRECTION ( 'NONE',  ( 0.000000000000000000, 0.000000000000000000, 1.000000000000000000 ) ) ;
#5831 = VERTEX_POINT ( 'NONE', #17766 ) ;
#5832 = DIRECTION ( 'NONE',  ( 0.000000000000000000, 0.000000000000000000, 1.000000000000000000 ) ) ;
#5833 = VERTEX_POINT ( 'NONE', #1674 ) ;
#5834 = DIRECTION ( 'NONE',  ( -0.000000000000000000, -1.000000000000000000, -0.000000000000000000 ) ) ;
#5835 = CARTESIAN_POINT ( 'NONE',  ( 10.00000000000000000, -16.10733642026445978, -53.89344778774828626 ) ) ;
#5836 = ORIENTED_EDGE ( 'NONE', *, *, #8067, .F. ) ;
#5837 = SHAPE_DEFINITION_REPRESENTATION ( #17121, #8256 ) ;
#5838 = ADVANCED_FACE ( 'NONE', ( #16249, #15112 ), #3487, .F. ) ;
#5839 = EDGE_LOOP ( 'NONE', ( #17998, #15562, #761, #1004, #5794 ) ) ;
#5840 = CIRCLE ( 'NONE', #16486, 24.00000000002399503 ) ;
#5841 = ORIENTED_EDGE ( 'NONE', *, *, #3655, .F. ) ;
#5842 = DIRECTION ( 'NONE',  ( 0.000000000000000000, 0.000000000000000000, -1.000000000000000000 ) ) ;
#5843 = DIRECTION ( 'NONE',  ( -1.000000000000000000, 0.000000000000000000, -0.000000000000000000 ) ) ;
#5844 = DIRECTION ( 'NONE',  ( 0.000000000000000000, 0.000000000000000000, 1.000000000000000000 ) ) ;
#5845 = DIRECTION ( 'NONE',  ( 0.000000000000000000, 0.000000000000000000, -1.000000000000000000 ) ) ;
#5846 = CARTESIAN_POINT ( 'NONE',  ( 10.00000000000000000, 24.68609584167159454, 50.69000562871650573 ) ) ;
#5847 = LINE ( 'NONE', #2617, #11519 ) ;
#5848 = EDGE_LOOP ( 'NONE', ( #11681, #17521, #4898, #7495 ) ) ;
#5849 = FACE_OUTER_BOUND ( 'NONE', #1086, .T. ) ;
#5850 = CARTESIAN_POINT ( 'NONE',  ( -36.40576474687247099, 0.000000000000000000, 23.80033635316149443 ) ) ;
#5851 = CARTESIAN_POINT ( 'NONE',  ( 0.000000000000000000, 1.178949249685218081, 2.041999999999998483 ) ) ;
#5852 = ORIENTED_EDGE ( 'NONE', *, *, #6643, .F. ) ;
#5853 = ORIENTED_EDGE ( 'NONE', *, *, #497, .T. ) ;
#5854 = EDGE_CURVE ( 'NONE', #15698, #3193, #15015, .T. ) ;
#5855 = EDGE_CURVE ( 'NONE', #15649, #6911, #255, .T. ) ;
#5856 = CARTESIAN_POINT ( 'NONE',  ( 0.000000000000000000, -41.62350880771954564, 47.29147401531940886 ) ) ;
#5857 = DIRECTION ( 'NONE',  ( 1.000000000000000000, 0.000000000000000000, 0.000000000000000000 ) ) ;
#5858 = EDGE_CURVE ( 'NONE', #1277, #10958, #1775, .T. ) ;
#5859 = EDGE_LOOP ( 'NONE', ( #13206, #4441, #5605 ) ) ;
#5860 = ADVANCED_FACE ( 'NONE', ( #16349 ), #4628, .T. ) ;
#5861 = PRODUCT_DEFINITION_SHAPE ( 'NONE', 'NONE',  #1543 ) ;
#5862 = EDGE_CURVE ( 'NONE', #18364, #10019, #5111, .T. ) ;
#5863 = AXIS2_PLACEMENT_3D ( 'NONE', #14361, #12934, #10164 ) ;
#5864 = DIRECTION ( 'NONE',  ( 0.000000000000000000, 0.000000000000000000, 1.000000000000000000 ) ) ;
#5865 = CARTESIAN_POINT ( 'NONE',  ( 10.00000000000000000, -46.27827401617427228, 31.97297851452409034 ) ) ;
#5866 = AXIS2_PLACEMENT_3D ( 'NONE', #2124, #7928, #1841 ) ;
#5867 = EDGE_CURVE ( 'NONE', #3467, #1784, #13040, .T. ) ;
#5868 = CIRCLE ( 'NONE', #8310, 2.649999999999997691 ) ;
#5869 = DIRECTION ( 'NONE',  ( 1.000000000000000000, 0.000000000000000000, 0.000000000000000000 ) ) ;
#5870 = ORIENTED_EDGE ( 'NONE', *, *, #5750, .T. ) ;
#5871 = FACE_BOUND ( 'NONE', #13970, .T. ) ;
#5872 = EDGE_CURVE ( 'NONE', #5739, #11098, #1477, .T. ) ;
#5873 = ORIENTED_EDGE ( 'NONE', *, *, #8293, .F. ) ;
#5874 = DIRECTION ( 'NONE',  ( 1.000000000000000000, 0.000000000000000000, 0.000000000000000000 ) ) ;
#5875 = VERTEX_POINT ( 'NONE', #12331 ) ;
#5876 = ORIENTED_EDGE ( 'NONE', *, *, #10525, .T. ) ;
#5877 = DIRECTION ( 'NONE',  ( 0.000000000000000000, -0.8660254037844390407, -0.4999999999999993339 ) ) ;
#5878 = DIRECTION ( 'NONE',  ( 1.000000000000000000, 0.000000000000000000, 0.000000000000000000 ) ) ;
#5879 = VERTEX_POINT ( 'NONE', #827 ) ;
#5880 = ORIENTED_EDGE ( 'NONE', *, *, #3896, .F. ) ;
#5881 = ADVANCED_FACE ( 'NONE', ( #5382 ), #2435, .T. ) ;
#5882 = LINE ( 'NONE', #4364, #13291 ) ;
#5883 = SURFACE_STYLE_FILL_AREA ( #8919 ) ;
#5884 = AXIS2_PLACEMENT_3D ( 'NONE', #17471, #8805, #8893 ) ;
#5885 = VERTEX_POINT ( 'NONE', #11189 ) ;
#5886 = DIRECTION ( 'NONE',  ( -1.000000000000000000, 0.000000000000000000, 0.000000000000000000 ) ) ;
#5887 = EDGE_CURVE ( 'NONE', #18040, #10550, #16731, .T. ) ;
#5888 = DIRECTION ( 'NONE',  ( -0.000000000000000000, 1.000000000000000000, -0.000000000000000000 ) ) ;
#5889 = ORIENTED_EDGE ( 'NONE', *, *, #10342, .F. ) ;
#5890 = AXIS2_PLACEMENT_3D ( 'NONE', #16026, #2990, #8787 ) ;
#5891 = ORIENTED_EDGE ( 'NONE', *, *, #10405, .F. ) ;
#5892 = CARTESIAN_POINT ( 'NONE',  ( 0.000000000000000000, 0.000000000000000000, 0.000000000000000000 ) ) ;
#5893 = DIRECTION ( 'NONE',  ( -1.000000000000000000, 0.000000000000000000, 0.000000000000000000 ) ) ;
#5894 = CARTESIAN_POINT ( 'NONE',  ( 5.000000000000000000, 54.20017844242511273, 32.11449294037214486 ) ) ;
#5895 = EDGE_LOOP ( 'NONE', ( #8114, #3787 ) ) ;
#5896 = DIRECTION ( 'NONE',  ( 0.9938152567191714803, 0.000000000000000000, -0.1110460963393456596 ) ) ;
#5897 = FACE_OUTER_BOUND ( 'NONE', #13495, .T. ) ;
#5898 = LINE ( 'NONE', #4472, #8601 ) ;
#5899 = LINE ( 'NONE', #11712, #13870 ) ;
#5900 = ORIENTED_EDGE ( 'NONE', *, *, #17692, .F. ) ;
#5901 = DIRECTION ( 'NONE',  ( -1.000000000000000000, 0.000000000000000000, 0.000000000000000000 ) ) ;
#5902 = CYLINDRICAL_SURFACE ( 'NONE', #1119, 12.00000000001200462 ) ;
#5903 = ORIENTED_EDGE ( 'NONE', *, *, #1687, .T. ) ;
#5904 = CARTESIAN_POINT ( 'NONE',  ( 0.000000000000000000, 0.000000000000000000, 0.000000000000000000 ) ) ;
#5905 = CARTESIAN_POINT ( 'NONE',  ( 10.00000000000000000, 0.000000000000000000, 0.000000000000000000 ) ) ;
#5906 = ADVANCED_FACE ( 'NONE', ( #4995 ), #15470, .F. ) ;
#5907 = ORIENTED_EDGE ( 'NONE', *, *, #456, .F. ) ;
#5908 = CARTESIAN_POINT ( 'NONE',  ( 5.686050877451574337, -5.768780236673276995, 0.000000000000000000 ) ) ;
#5909 = DIRECTION ( 'NONE',  ( 0.000000000000000000, 0.000000000000000000, 1.000000000000000000 ) ) ;
#5910 = ORIENTED_EDGE ( 'NONE', *, *, #18159, .T. ) ;
#5911 = CARTESIAN_POINT ( 'NONE',  ( 0.000000000000000000, 24.46385708179996854, -9.514709542736643044 ) ) ;
#5912 = DIRECTION ( 'NONE',  ( -0.000000000000000000, 1.000000000000000000, -0.000000000000000000 ) ) ;
#5913 = DIRECTION ( 'NONE',  ( 1.000000000000000000, 0.000000000000000000, 0.000000000000000000 ) ) ;
#5914 = DIRECTION ( 'NONE',  ( 0.000000000000000000, 1.000000000000000000, 0.000000000000000000 ) ) ;
#5915 = VERTEX_POINT ( 'NONE', #12526 ) ;
#5916 = DIRECTION ( 'NONE',  ( 0.000000000000000000, 0.000000000000000000, 1.000000000000000000 ) ) ;
#5917 = ORIENTED_EDGE ( 'NONE', *, *, #13158, .T. ) ;
#5918 = EDGE_CURVE ( 'NONE', #1626, #10049, #15575, .T. ) ;
#5919 = DIRECTION ( 'NONE',  ( -1.000000000000000000, 0.000000000000000000, 0.000000000000000000 ) ) ;
#5920 = ORIENTED_EDGE ( 'NONE', *, *, #9888, .F. ) ;
#5921 = APPLICATION_PROTOCOL_DEFINITION ( 'draft international standard', 'automotive_design', 1998, #1115 ) ;
#5922 = ADVANCED_FACE ( 'NONE', ( #8340 ), #4816, .T. ) ;
#5923 = EDGE_LOOP ( 'NONE', ( #18774, #15797, #8179, #5221 ) ) ;
#5924 = AXIS2_PLACEMENT_3D ( 'NONE', #13505, #17882, #10642 ) ;
#5925 = AXIS2_PLACEMENT_3D ( 'NONE', #15881, #232, #6034 ) ;
#5926 = DIRECTION ( 'NONE',  ( 0.000000000000000000, 1.000000000000000000, 0.000000000000000000 ) ) ;
#5927 = DIRECTION ( 'NONE',  ( 0.000000000000000000, -0.9510565162951565288, 0.3090169943749384029 ) ) ;
#5928 = DIRECTION ( 'NONE',  ( -1.000000000000000000, 0.000000000000000000, -0.000000000000000000 ) ) ;
#5929 = DIRECTION ( 'NONE',  ( 0.000000000000000000, 1.000000000000000000, 0.000000000000000000 ) ) ;
#5930 = DIRECTION ( 'NONE',  ( 0.000000000000000000, -0.3090169943749350723, -0.9510565162951576390 ) ) ;
#5931 = LINE ( 'NONE', #7024, #2205 ) ;
#5932 = CARTESIAN_POINT ( 'NONE',  ( 0.000000000000000000, 39.14194549634421350, -40.58063702438301590 ) ) ;
#5933 = VERTEX_POINT ( 'NONE', #14052 ) ;
#5934 = ORIENTED_EDGE ( 'NONE', *, *, #15467, .T. ) ;
#5935 = CARTESIAN_POINT ( 'NONE',  ( 0.000000000000000000, 62.87238730325621106, -4.007856633823609016 ) ) ;
#5936 = CARTESIAN_POINT ( 'NONE',  ( 2.500000000000000000, -1.178949249685218748, -2.041999999999998039 ) ) ;
#5937 = ORIENTED_EDGE ( 'NONE', *, *, #291, .F. ) ;
#5938 = CIRCLE ( 'NONE', #7463, 24.00000000002400569 ) ;
#5939 = ORIENTED_EDGE ( 'NONE', *, *, #917, .F. ) ;
#5940 = CIRCLE ( 'NONE', #10509, 56.24900000005625600 ) ;
#5941 = DIRECTION ( 'NONE',  ( 0.000000000000000000, -6.982962677686266711E-15, 1.000000000000000000 ) ) ;
#5942 = DIRECTION ( 'NONE',  ( 0.000000000000000000, 0.000000000000000000, 1.000000000000000000 ) ) ;
#5943 = ORIENTED_EDGE ( 'NONE', *, *, #5246, .F. ) ;
#5944 = VECTOR ( 'NONE', #10913, 1000.000000000000000 ) ;
#5945 = AXIS2_PLACEMENT_3D ( 'NONE', #14201, #2394, #8209 ) ;
#5946 = LINE ( 'NONE', #8449, #15377 ) ;
#5947 = CARTESIAN_POINT ( 'NONE',  ( 34.99999999999999289, 2.516649172247811061E-16, -2.055000000000000160 ) ) ;
#5948 = AXIS2_PLACEMENT_3D ( 'NONE', #8035, #2142, #1005 ) ;
#5950 = CIRCLE ( 'NONE', #8399, 63.00000000006298961 ) ;
#5949 = FACE_OUTER_BOUND ( 'NONE', #13108, .T. ) ;
#5951 = ORIENTED_EDGE ( 'NONE', *, *, #3704, .F. ) ;
#5952 = ADVANCED_FACE ( 'NONE', ( #2332 ), #12241, .F. ) ;
#5953 = DIRECTION ( 'NONE',  ( 0.000000000000000000, 0.000000000000000000, 1.000000000000000000 ) ) ;
#5954 = EDGE_CURVE ( 'NONE', #15928, #13348, #1173, .T. ) ;
#5955 = ORIENTED_EDGE ( 'NONE', *, *, #7794, .F. ) ;
#5956 = CARTESIAN_POINT ( 'NONE',  ( 10.00000000000000000, 14.19907017806868588, 22.07705612348844326 ) ) ;
#5957 = ORIENTED_EDGE ( 'NONE', *, *, #619, .T. ) ;
#5958 = ORIENTED_EDGE ( 'NONE', *, *, #1863, .F. ) ;
#5959 = EDGE_CURVE ( 'NONE', #17584, #17410, #8471, .T. ) ;
#5960 = DIRECTION ( 'NONE',  ( 1.000000000000000000, 0.000000000000000000, 0.000000000000000000 ) ) ;
#5961 = DIRECTION ( 'NONE',  ( 0.000000000000000000, 0.9876883405951382144, -0.1564344650402274828 ) ) ;
#5962 = AXIS2_PLACEMENT_3D ( 'NONE', #6328, #13481, #423 ) ;
#5963 = ORIENTED_EDGE ( 'NONE', *, *, #7952, .T. ) ;
#5964 = ORIENTED_EDGE ( 'NONE', *, *, #7124, .F. ) ;
#5965 = AXIS2_PLACEMENT_3D ( 'NONE', #2093, #14951, #17707 ) ;
#5966 = DIRECTION ( 'NONE',  ( 0.000000000000000000, 1.000000000000000000, 0.000000000000000000 ) ) ;
#5967 = EDGE_CURVE ( 'NONE', #10934, #11971, #9989, .T. ) ;
#5968 = ORIENTED_EDGE ( 'NONE', *, *, #9689, .T. ) ;
#5969 = CYLINDRICAL_SURFACE ( 'NONE', #14565, 26.24900000002624978 ) ;
#5970 = CIRCLE ( 'NONE', #8416, 41.00000000000000000 ) ;
#5971 = AXIS2_PLACEMENT_3D ( 'NONE', #3771, #15211, #2063 ) ;
#5972 = EDGE_CURVE ( 'NONE', #12239, #2843, #1764, .T. ) ;
#5973 = CARTESIAN_POINT ( 'NONE',  ( -117.1020693116508085, -30.00000000000000000, 17.04080595179779678 ) ) ;
#5974 = AXIS2_PLACEMENT_3D ( 'NONE', #1974, #12072, #11883 ) ;
#5975 = ORIENTED_EDGE ( 'NONE', *, *, #12831, .F. ) ;
#5976 = EDGE_CURVE ( 'NONE', #18009, #14803, #3914, .T. ) ;
#5977 = CIRCLE ( 'NONE', #16634, 27.00000000000000355 ) ;
#5978 = ADVANCED_FACE ( 'NONE', ( #15291 ), #13853, .F. ) ;
#5979 = CIRCLE ( 'NONE', #15734, 2.500000000000000888 ) ;
#5980 = ORIENTED_EDGE ( 'NONE', *, *, #14420, .T. ) ;
#5981 = CARTESIAN_POINT ( 'NONE',  ( 0.000000000000000000, 50.69000562871642046, -24.68609584167177218 ) ) ;
#5982 = FACE_OUTER_BOUND ( 'NONE', #17091, .T. ) ;
#5983 = FACE_OUTER_BOUND ( 'NONE', #17709, .T. ) ;
#5984 = VERTEX_POINT ( 'NONE', #18245 ) ;
#5985 = CYLINDRICAL_SURFACE ( 'NONE', #13306, 2.649999999999999467 ) ;
#5986 = EDGE_CURVE ( 'NONE', #12173, #5480, #5732, .T. ) ;
#5987 = CARTESIAN_POINT ( 'NONE',  ( 10.00000000000000000, -53.89344778774823652, 16.10733642026462675 ) ) ;
#5988 = CYLINDRICAL_SURFACE ( 'NONE', #9180, 56.24900000005625600 ) ;
#5989 = DIRECTION ( 'NONE',  ( 0.000000000000000000, 1.000000000000000000, -1.287488025362403787E-15 ) ) ;
#5990 = ORIENTED_EDGE ( 'NONE', *, *, #9335, .T. ) ;
#5991 = CARTESIAN_POINT ( 'NONE',  ( 21.00000000000000355, 0.000000000000000000, 2.055000000000000160 ) ) ;
#5992 = EDGE_CURVE ( 'NONE', #17369, #72, #16669, .T. ) ;
#5993 = ORIENTED_EDGE ( 'NONE', *, *, #2483, .T. ) ;
#5994 = CARTESIAN_POINT ( 'NONE',  ( 10.00000000000000000, 16.10733642026482570, 53.89344778774818678 ) ) ;
#5995 = FACE_BOUND ( 'NONE', #10950, .T. ) ;
#5996 = AXIS2_PLACEMENT_3D ( 'NONE', #1520, #15553, #9 ) ;
#5997 = CIRCLE ( 'NONE', #545, 12.00000000001200284 ) ;
#5998 = AXIS2_PLACEMENT_3D ( 'NONE', #11012, #5118, #13786 ) ;
#5999 = ORIENTED_EDGE ( 'NONE', *, *, #9203, .T. ) ;
#6000 = CARTESIAN_POINT ( 'NONE',  ( 11.14999999999999680, 0.000000000000000000, 0.000000000000000000 ) ) ;
#6001 = DIRECTION ( 'NONE',  ( -1.000000000000000000, 0.000000000000000000, 0.000000000000000000 ) ) ;
#6002 = AXIS2_PLACEMENT_3D ( 'NONE', #6263, #17891, #4845 ) ;
#6003 = VERTEX_POINT ( 'NONE', #15487 ) ;
#6004 = CARTESIAN_POINT ( 'NONE',  ( -6.259644161404859044E-16, -4.618802153517026277, -3.504271511727133248 ) ) ;
#6005 = DIRECTION ( 'NONE',  ( 1.000000000000000000, 0.000000000000000000, 0.000000000000000000 ) ) ;
#6006 = CIRCLE ( 'NONE', #9051, 24.00000000002399858 ) ;
#6007 = CARTESIAN_POINT ( 'NONE',  ( 10.00000000000000000, 0.000000000000000000, 0.000000000000000000 ) ) ;
#6008 = FACE_OUTER_BOUND ( 'NONE', #3493, .T. ) ;
#6009 = DIRECTION ( 'NONE',  ( 0.000000000000000000, 0.000000000000000000, 1.000000000000000000 ) ) ;
#6010 = VERTEX_POINT ( 'NONE', #13005 ) ;
#6011 = AXIS2_PLACEMENT_3D ( 'NONE', #12503, #11161, #2411 ) ;
#6012 = CARTESIAN_POINT ( 'NONE',  ( 4.078421086530217288, -3.990950201428958621, -1.000000000000000000 ) ) ;
#6013 = VERTEX_POINT ( 'NONE', #5667 ) ;
#6014 = EDGE_CURVE ( 'NONE', #15251, #6022, #15666, .T. ) ;
#6015 = PRODUCT_DEFINITION_SHAPE ( 'NONE', 'NONE',  #18826 ) ;
#6016 = CARTESIAN_POINT ( 'NONE',  ( -4.204015924366189871, 1.626724848190922446, -3.610627190413390419 ) ) ;
#6017 = VERTEX_POINT ( 'NONE', #1478 ) ;
#6018 = B_SPLINE_CURVE_WITH_KNOTS ( 'NONE', 3,
 ( #17788, #4741, #16376, #3334, #6266, #13614 ),
 .UNSPECIFIED., .F., .F.,
 ( 4, 2, 4 ),
 ( -3.640115492407174633E-06, 0.0002066546034003413743, 0.0004169493222930899571 ),
 .UNSPECIFIED. ) ;
#6019 = ORIENTED_EDGE ( 'NONE', *, *, #10677, .F. ) ;
#6020 = AXIS2_PLACEMENT_3D ( 'NONE', #9104, #16160, #4826 ) ;
#6021 = AXIS2_PLACEMENT_3D ( 'NONE', #683, #2109, #8210 ) ;
#6022 = VERTEX_POINT ( 'NONE', #4152 ) ;
#6023 = AXIS2_PLACEMENT_3D ( 'NONE', #12980, #5741, #7253 ) ;
#6024 = CIRCLE ( 'NONE', #8764, 24.00000000002399503 ) ;
#6025 = EDGE_CURVE ( 'NONE', #7169, #5282, #5430, .T. ) ;
#6026 = CARTESIAN_POINT ( 'NONE',  ( 0.000000000000000000, 0.000000000000000000, 0.000000000000000000 ) ) ;
#6027 = CARTESIAN_POINT ( 'NONE',  ( 3.999999999999999112, 2.309401076758497595, -3.504271511727124366 ) ) ;
#6028 = FACE_OUTER_BOUND ( 'NONE', #14859, .T. ) ;
#6029 = FACE_OUTER_BOUND ( 'NONE', #13420, .T. ) ;
#6030 = EDGE_CURVE ( 'NONE', #6186, #12797, #3296, .T. ) ;
#6031 = CYLINDRICAL_SURFACE ( 'NONE', #13906, 12.00000000001200107 ) ;
#6032 = AXIS2_PLACEMENT_3D ( 'NONE', #15858, #13102, #2808 ) ;
#6033 = CYLINDRICAL_SURFACE ( 'NONE', #1599, 24.00000000002400213 ) ;
#6034 = DIRECTION ( 'NONE',  ( 0.000000000000000000, 0.000000000000000000, 1.000000000000000000 ) ) ;
#6035 = DIRECTION ( 'NONE',  ( 1.000000000000000000, 0.000000000000000000, 0.000000000000000000 ) ) ;
#6036 = ORIENTED_EDGE ( 'NONE', *, *, #270, .F. ) ;
#6037 = VECTOR ( 'NONE', #12779, 1000.000000000000000 ) ;
#6038 = CARTESIAN_POINT ( 'NONE',  ( -90.67999921423555065, 1.000000000000018208, -4.751589320297106234 ) ) ;
#6039 = CARTESIAN_POINT ( 'NONE',  ( 10.00000000000000000, -53.92768374110879392, -16.45250512421912603 ) ) ;
#6040 = CARTESIAN_POINT ( 'NONE',  ( -4.888507282057958037, -29.45674523562211888, 0.000000000000000000 ) ) ;
#6041 = CIRCLE ( 'NONE', #14569, 2.649999999999992806 ) ;
#6042 = VERTEX_POINT ( 'NONE', #4059 ) ;
#6043 = VERTEX_POINT ( 'NONE', #14334 ) ;
#6044 = CIRCLE ( 'NONE', #13043, 20.00000000000000000 ) ;
#6045 = CARTESIAN_POINT ( 'NONE',  ( 0.000000000000000000, 4.381479206523448688, -32.70783759231082399 ) ) ;
#6046 = FILL_AREA_STYLE ('',( #10059 ) ) ;
#6047 = DIRECTION ( 'NONE',  ( -0.000000000000000000, -1.000000000000000000, -0.000000000000000000 ) ) ;
#6048 = ORIENTED_EDGE ( 'NONE', *, *, #17158, .F. ) ;
#6049 = CIRCLE ( 'NONE', #3812, 6.080745460913608902 ) ;
#6050 = EDGE_CURVE ( 'NONE', #9528, #4173, #7004, .T. ) ;
#6051 = CIRCLE ( 'NONE', #13066, 24.00000000002399858 ) ;
#6052 = CARTESIAN_POINT ( 'NONE',  ( -90.67999921423555065, 1.000000000000018208, -4.751589320297106234 ) ) ;
#6053 = DIRECTION ( 'NONE',  ( -1.000000000000000000, -0.000000000000000000, -0.000000000000000000 ) ) ;
#6054 = CARTESIAN_POINT ( 'NONE',  ( 2.500000000000000000, -1.178949249685214307, 2.042000000000001592 ) ) ;
#6055 = ORIENTED_EDGE ( 'NONE', *, *, #9841, .T. ) ;
#6056 = CARTESIAN_POINT ( 'NONE',  ( 0.6507732100473444525, -4.243078065514795050, -0.2236248678334952777 ) ) ;
#6057 = EDGE_CURVE ( 'NONE', #4502, #16169, #10283, .T. ) ;
#6058 = VERTEX_POINT ( 'NONE', #15945 ) ;
#6059 = DIRECTION ( 'NONE',  ( 0.03086419753086420623, 0.9995235871707959241, -0.000000000000000000 ) ) ;
#6060 = ORIENTED_EDGE ( 'NONE', *, *, #10968, .T. ) ;
#6061 = CARTESIAN_POINT ( 'NONE',  ( 0.000000000000000000, -30.00000000000000000, 0.000000000000000000 ) ) ;
#6062 = CARTESIAN_POINT ( 'NONE',  ( 3.511755186886750923, -2.826662030176382956, -3.597382984111582083 ) ) ;
#6063 = AXIS2_PLACEMENT_3D ( 'NONE', #16187, #17, #9034 ) ;
#6064 = ORIENTED_EDGE ( 'NONE', *, *, #8679, .F. ) ;
#6065 = EDGE_LOOP ( 'NONE', ( #1973, #9461 ) ) ;
#6066 = CARTESIAN_POINT ( 'NONE',  ( 10.04305231718579705, -26.50000000000000000, 28.25933677959249835 ) ) ;
#6067 = VECTOR ( 'NONE', #18256, 1000.000000000000000 ) ;
#6068 = SURFACE_SIDE_STYLE ('',( #7400 ) ) ;
#6069 = ORIENTED_EDGE ( 'NONE', *, *, #8644, .F. ) ;
#6070 = LINE ( 'NONE', #18809, #3630 ) ;
#6071 = ADVANCED_FACE ( 'NONE', ( #17195 ), #1203, .F. ) ;
#6072 = EDGE_CURVE ( 'NONE', #7904, #4042, #10230, .T. ) ;
#6073 = DIRECTION ( 'NONE',  ( 0.9938152567191715914, 0.000000000000000000, -0.1110460963393456735 ) ) ;
#6074 = AXIS2_PLACEMENT_3D ( 'NONE', #15692, #17046, #3989 ) ;
#6075 = VERTEX_POINT ( 'NONE', #14614 ) ;
#6076 = MECHANICAL_DESIGN_GEOMETRIC_PRESENTATION_REPRESENTATION (  '', ( #17339 ), #17048 ) ;
#6077 = EDGE_LOOP ( 'NONE', ( #10014, #4213 ) ) ;
#6078 = PLANE ( 'NONE',  #16629 ) ;
#6079 = CYLINDRICAL_SURFACE ( 'NONE', #18392, 28.00000000000000355 ) ;
#6080 = CYLINDRICAL_SURFACE ( 'NONE', #13302, 2.649999999999999467 ) ;
#6081 = ORIENTED_EDGE ( 'NONE', *, *, #11280, .T. ) ;
#6082 = DIRECTION ( 'NONE',  ( 0.000000000000000000, 1.000000000000000000, -1.103561164596346103E-15 ) ) ;
#6083 = EDGE_CURVE ( 'NONE', #17080, #195, #5847, .T. ) ;
#6084 = CARTESIAN_POINT ( 'NONE',  ( -10.00000000000000000, 0.000000000000000000, 0.000000000000000000 ) ) ;
#6085 = CARTESIAN_POINT ( 'NONE',  ( 0.000000000000000000, 50.71018745830478736, -24.33982105418846942 ) ) ;
#6086 = DIRECTION ( 'NONE',  ( 1.000000000000000000, -0.000000000000000000, -0.000000000000000000 ) ) ;
#6087 = ORIENTED_EDGE ( 'NONE', *, *, #18201, .F. ) ;
#6088 = DIRECTION ( 'NONE',  ( -1.000000000000000000, 0.000000000000000000, 0.000000000000000000 ) ) ;
#6089 = CARTESIAN_POINT ( 'NONE',  ( 3.673940397442059178E-15, 10.00000000000000000, 30.00000000000000000 ) ) ;
#6090 = ORIENTED_EDGE ( 'NONE', *, *, #11169, .F. ) ;
#6091 = DIRECTION ( 'NONE',  ( -1.000000000000000000, -0.000000000000000000, -0.000000000000000000 ) ) ;
#6092 = CARTESIAN_POINT ( 'NONE',  ( -90.00000000009001155, -29.99899999999999878, 10.00000000000000711 ) ) ;
#6093 = EDGE_CURVE ( 'NONE', #18364, #16450, #7179, .T. ) ;
#6094 = VECTOR ( 'NONE', #12497, 999.9999999999998863 ) ;
#6095 = EDGE_CURVE ( 'NONE', #13907, #12788, #8165, .T. ) ;
#6096 = ADVANCED_FACE ( 'NONE', ( #17108, #10048 ), #9954, .F. ) ;
#6097 = EDGE_CURVE ( 'NONE', #833, #10933, #8182, .T. ) ;
#6098 = ORIENTED_EDGE ( 'NONE', *, *, #18368, .T. ) ;
#6099 = CARTESIAN_POINT ( 'NONE',  ( 2.500000000000000000, -1.178949249685214307, 2.042000000000001592 ) ) ;
#6100 = DIRECTION ( 'NONE',  ( 0.000000000000000000, 0.000000000000000000, -1.000000000000000000 ) ) ;
#6101 = ORIENTED_EDGE ( 'NONE', *, *, #2162, .F. ) ;
#6102 = CYLINDRICAL_SURFACE ( 'NONE', #13961, 26.24900000002624978 ) ;
#6103 =( REPRESENTATION_RELATIONSHIP ('NONE','NONE', #11014, #18682 ) REPRESENTATION_RELATIONSHIP_WITH_TRANSFORMATION ( #39 )SHAPE_REPRESENTATION_RELATIONSHIP( ) );
#6104 = LINE ( 'NONE', #17364, #17242 ) ;
#6105 = ADVANCED_FACE ( 'NONE', ( #16044 ), #5769, .T. ) ;
#6106 = CARTESIAN_POINT ( 'NONE',  ( 0.000000000000000000, 0.000000000000000000, -2.000000000000000000 ) ) ;
#6107 = DIRECTION ( 'NONE',  ( -1.000000000000000000, 0.000000000000000000, 0.000000000000000000 ) ) ;
#6108 = DIRECTION ( 'NONE',  ( -1.000000000000000000, 0.000000000000000000, 0.000000000000000000 ) ) ;
#6109 = EDGE_LOOP ( 'NONE', ( #12115, #2874 ) ) ;
#6110 = CARTESIAN_POINT ( 'NONE',  ( 0.000000000000000000, 0.000000000000000000, 0.000000000000000000 ) ) ;
#6111 = ORIENTED_EDGE ( 'NONE', *, *, #18132, .F. ) ;
#6112 = DIRECTION ( 'NONE',  ( -1.000000000000000000, 0.000000000000000000, 0.000000000000000000 ) ) ;
#6113 = ORIENTED_EDGE ( 'NONE', *, *, #57, .T. ) ;
#6114 = EDGE_CURVE ( 'NONE', #5754, #17080, #17014, .T. ) ;
#6115 = ITEM_DEFINED_TRANSFORMATION ( 'NONE', 'NONE', #1968,  #8017 ) ;
#6116 = ORIENTED_EDGE ( 'NONE', *, *, #4263, .T. ) ;
#6117 = CIRCLE ( 'NONE', #11894, 12.00000000001200284 ) ;
#6118 = ORIENTED_EDGE ( 'NONE', *, *, #9581, .F. ) ;
#6119 = EDGE_CURVE ( 'NONE', #18371, #8784, #14558, .T. ) ;
#6120 = ORIENTED_EDGE ( 'NONE', *, *, #303, .T. ) ;
#6121 = DIRECTION ( 'NONE',  ( 0.000000000000000000, 0.000000000000000000, 1.000000000000000000 ) ) ;
#6122 = DIRECTION ( 'NONE',  ( -0.000000000000000000, 1.000000000000000000, -0.000000000000000000 ) ) ;
#6123 = CARTESIAN_POINT ( 'NONE',  ( -36.40576474687271258, 10.00000000000000000, -23.80033635316118890 ) ) ;
#6124 = DIRECTION ( 'NONE',  ( -1.000000000000000000, -0.000000000000000000, 0.000000000000000000 ) ) ;
#6125 = CYLINDRICAL_SURFACE ( 'NONE', #530, 12.00000000001200462 ) ;
#6126 = CYLINDRICAL_SURFACE ( 'NONE', #14673, 2.649999999999999467 ) ;
#6127 = CARTESIAN_POINT ( 'NONE',  ( 3.333333333333332593, 2.694301256218250007, -3.300726591567078483 ) ) ;
#6128 = CARTESIAN_POINT ( 'NONE',  ( 10.00000000000000000, 24.46385708179984064, 9.514709542736980552 ) ) ;
#6129 = EDGE_LOOP ( 'NONE', ( #5701, #11141, #6120, #9815 ) ) ;
#6130 = FILL_AREA_STYLE_COLOUR ( '', #18419 ) ;
#6131 = CARTESIAN_POINT ( 'NONE',  ( 10.00000000000000000, 46.27827401617449965, -31.97297851452373507 ) ) ;
#6132 = LINE ( 'NONE', #10420, #13014 ) ;
#6133 = ORIENTED_EDGE ( 'NONE', *, *, #8375, .T. ) ;
#6134 = ORIENTED_EDGE ( 'NONE', *, *, #3346, .F. ) ;
#6135 = CARTESIAN_POINT ( 'NONE',  ( -3.355112389629170799, 2.681727112203152963, -0.2256878752776689534 ) ) ;
#6136 = DIRECTION ( 'NONE',  ( 0.000000000000000000, 0.000000000000000000, 1.000000000000000000 ) ) ;
#6137 = VECTOR ( 'NONE', #2788, 1000.000000000000000 ) ;
#6138 = CARTESIAN_POINT ( 'NONE',  ( -23.50000000000000355, 2.877919977996280715E-15, 0.000000000000000000 ) ) ;
#6139 = ORIENTED_EDGE ( 'NONE', *, *, #4101, .T. ) ;
#6140 = EDGE_CURVE ( 'NONE', #560, #11392, #15481, .T. ) ;
#6141 = AXIS2_PLACEMENT_3D ( 'NONE', #242, #425, #2757 ) ;
#6142 = CARTESIAN_POINT ( 'NONE',  ( 10.00000000000000000, 56.37237871411034007, 1.017308535512583711 ) ) ;
#6143 = DIRECTION ( 'NONE',  ( -0.9995235871707960351, -0.03086419753086420970, 0.000000000000000000 ) ) ;
#6144 = CYLINDRICAL_SURFACE ( 'NONE', #9041, 24.00000000002399858 ) ;
#6145 = ORIENTED_EDGE ( 'NONE', *, *, #18432, .T. ) ;
#6146 = LINE ( 'NONE', #13204, #7038 ) ;
#6147 = VECTOR ( 'NONE', #15625, 1000.000000000000000 ) ;
#6148 = ORIENTED_EDGE ( 'NONE', *, *, #13257, .F. ) ;
#6149 = UNCERTAINTY_MEASURE_WITH_UNIT (LENGTH_MEASURE( 1.000000000000000082E-05 ), #9900, 'distance_accuracy_value', 'NONE');
#6150 = CARTESIAN_POINT ( 'NONE',  ( -87.76214430591549842, -14.11572627500821042, 4.471241649927994111 ) ) ;
#6151 = EDGE_LOOP ( 'NONE', ( #16624, #4682, #12184, #4714 ) ) ;
#6152 = DIRECTION ( 'NONE',  ( 0.000000000000000000, 1.000000000000000000, 0.000000000000000000 ) ) ;
#6153 = CARTESIAN_POINT ( 'NONE',  ( -3.455068668934486276, 2.624017327439035707, -3.316620875263955437 ) ) ;
#6154 = ORIENTED_EDGE ( 'NONE', *, *, #2162, .T. ) ;
#6155 = ORIENTED_EDGE ( 'NONE', *, *, #14448, .F. ) ;
#6156 = EDGE_CURVE ( 'NONE', #13103, #432, #16691, .T. ) ;
#6157 = CARTESIAN_POINT ( 'NONE',  ( -26.29305231718584324, -30.00000000000000000, 21.75302069950530637 ) ) ;
#6158 = ORIENTED_EDGE ( 'NONE', *, *, #13486, .F. ) ;
#6159 = DIRECTION ( 'NONE',  ( 0.000000000000000000, 0.000000000000000000, 1.000000000000000000 ) ) ;
#6160 = ADVANCED_FACE ( 'NONE', ( #6319 ), #16231, .T. ) ;
#6161 = AXIS2_PLACEMENT_3D ( 'NONE', #9596, #11402, #4083 ) ;
#6162 = AXIS2_PLACEMENT_3D ( 'NONE', #9836, #5069, #904 ) ;
#6163 = VECTOR ( 'NONE', #8667, 1000.000000000000000 ) ;
#6164 = CARTESIAN_POINT ( 'NONE',  ( -4.154094228333542915, 2.398367420968061658, -3.721909803043254694 ) ) ;
#6165 = EDGE_LOOP ( 'NONE', ( #7775, #7846, #9694, #17374 ) ) ;
#6166 = PRODUCT_DEFINITION_SHAPE ( 'NONE', 'NONE',  #18813 ) ;
#6167 = ORIENTED_EDGE ( 'NONE', *, *, #15585, .T. ) ;
#6168 = LINE ( 'NONE', #11972, #1448 ) ;
#6169 = DIRECTION ( 'NONE',  ( 0.000000000000000000, 0.000000000000000000, -1.000000000000000000 ) ) ;
#6170 = CARTESIAN_POINT ( 'NONE',  ( 10.00000000000000000, -61.47135697633768814, -13.79392154159200068 ) ) ;
#6171 = ORIENTED_EDGE ( 'NONE', *, *, #9344, .F. ) ;
#6172 = CARTESIAN_POINT ( 'NONE',  ( 10.00000000000000000, 12.18267823974751352, 25.42247726998019530 ) ) ;
#6173 = CIRCLE ( 'NONE', #9227, 20.00000000000000000 ) ;
#6174 = DIRECTION ( 'NONE',  ( 0.01644736842105263067, -0.9998647328874151752, 0.000000000000000000 ) ) ;
#6175 = CARTESIAN_POINT ( 'NONE',  ( 0.000000000000000000, -61.47135697633788709, 13.79392154159114448 ) ) ;
#6176 = PLANE ( 'NONE',  #11135 ) ;
#6177 = VERTEX_POINT ( 'NONE', #1843 ) ;
#6178 = CIRCLE ( 'NONE', #16833, 2.649999999999999467 ) ;
#6179 = CARTESIAN_POINT ( 'NONE',  ( -26.29305231718584324, -26.50000000000000000, 19.10302069950530779 ) ) ;
#6180 = DIRECTION ( 'NONE',  ( -1.000000000000000000, 0.000000000000000000, 0.000000000000000000 ) ) ;
#6181 = ORIENTED_EDGE ( 'NONE', *, *, #10749, .T. ) ;
#6182 = DIRECTION ( 'NONE',  ( -1.000000000000000000, 0.000000000000000000, -0.000000000000000000 ) ) ;
#6183 = CARTESIAN_POINT ( 'NONE',  ( 0.000000000000000000, 13.24999999999999822, 0.000000000000000000 ) ) ;
#6184 = B_SPLINE_CURVE_WITH_KNOTS ( 'NONE', 3,
 ( #4850, #10655, #6464, #18076 ),
 .UNSPECIFIED., .F., .F.,
 ( 4, 4 ),
 ( 0.000000000000000000, 0.002452478801916361129 ),
 .UNSPECIFIED. ) ;
#6185 = AXIS2_PLACEMENT_3D ( 'NONE', #1084, #16891, #12309 ) ;
#6186 = VERTEX_POINT ( 'NONE', #12126 ) ;
#6187 = LINE ( 'NONE', #5208, #5194 ) ;
#6188 = VERTEX_POINT ( 'NONE', #7365 ) ;
#6189 = CARTESIAN_POINT ( 'NONE',  ( 10.00000000000000000, 0.000000000000000000, 0.000000000000000000 ) ) ;
#6190 = ADVANCED_FACE ( 'NONE', ( #3374 ), #10330, .T. ) ;
#6191 = DIRECTION ( 'NONE',  ( 1.000000000000000000, 0.000000000000000000, 0.000000000000000000 ) ) ;
#6192 = ADVANCED_FACE ( 'NONE', ( #13472 ), #4519, .T. ) ;
#6193 = EDGE_CURVE ( 'NONE', #3113, #7366, #7266, .T. ) ;
#6194 = DIRECTION ( 'NONE',  ( -0.000000000000000000, 1.000000000000000000, -0.000000000000000000 ) ) ;
#6195 = CARTESIAN_POINT ( 'NONE',  ( -117.1020693116506379, -30.00000000000000000, -22.34080595179800355 ) ) ;
#6196 = DIRECTION ( 'NONE',  ( -1.000000000000000000, -0.000000000000000000, -0.000000000000000000 ) ) ;
#6197 = ORIENTED_EDGE ( 'NONE', *, *, #2971, .F. ) ;
#6198 = CARTESIAN_POINT ( 'NONE',  ( 10.00000000000000000, -33.95787273855213328, -45.00825343885058061 ) ) ;
#6199 = EDGE_LOOP ( 'NONE', ( #17961, #17758, #9700, #6048 ) ) ;
#6200 = ADVANCED_FACE ( 'NONE', ( #13563 ), #16423, .T. ) ;
#6201 = SHAPE_REPRESENTATION_RELATIONSHIP ( 'NONE' , 'NONE' ,  #16742, #5356 ) ;
#6202 = LINE ( 'NONE', #10585, #7850 ) ;
#6203 = ORIENTED_EDGE ( 'NONE', *, *, #4631, .T. ) ;
#6204 = CONTEXT_DEPENDENT_SHAPE_REPRESENTATION ( #17188, #15897 ) ;
#6205 = EDGE_CURVE ( 'NONE', #7462, #8021, #1566, .T. ) ;
#6206 = ORIENTED_EDGE ( 'NONE', *, *, #6438, .T. ) ;
#6207 = ORIENTED_EDGE ( 'NONE', *, *, #11827, .F. ) ;
#6208 = EDGE_CURVE ( 'NONE', #8736, #13131, #11849, .T. ) ;
#6209 = EDGE_LOOP ( 'NONE', ( #14476, #3364, #17301, #6745 ) ) ;
#6210 = CARTESIAN_POINT ( 'NONE',  ( 0.000000000000000000, 40.58063702438344933, 39.14194549634378006 ) ) ;
#6211 = DIRECTION ( 'NONE',  ( -1.000000000000000000, -0.000000000000000000, -0.000000000000000000 ) ) ;
#6212 = LINE ( 'NONE', #1742, #11503 ) ;
#6213 = DIRECTION ( 'NONE',  ( 0.000000000000000000, -0.9510565162951499785, -0.3090169943749582204 ) ) ;
#6214 = EDGE_CURVE ( 'NONE', #7704, #2818, #10478, .T. ) ;
#6215 = ADVANCED_FACE ( 'NONE', ( #138 ), #10691, .F. ) ;
#6216 = CYLINDRICAL_SURFACE ( 'NONE', #18473, 26.24900000002624978 ) ;
#6217 = CARTESIAN_POINT ( 'NONE',  ( 10.00000000000000000, -1.335003989221234200, -56.23315539212691760 ) ) ;
#6218 = DIRECTION ( 'NONE',  ( 0.000000000000000000, 0.000000000000000000, 1.000000000000000000 ) ) ;
#6219 = CARTESIAN_POINT ( 'NONE',  ( -31.74999999999995737, 0.000000000000000000, 0.000000000000000000 ) ) ;
#6220 = ORIENTED_EDGE ( 'NONE', *, *, #2272, .T. ) ;
#6221 = CARTESIAN_POINT ( 'NONE',  ( 0.000000000000000000, 0.000000000000000000, -4.484454397937119197 ) ) ;
#6222 = CARTESIAN_POINT ( 'NONE',  ( 2.804994570502171047, 3.229033611042449792, -3.526374918436834704 ) ) ;
#6223 = DIRECTION ( 'NONE',  ( 0.000000000000000000, 0.000000000000000000, 1.000000000000000000 ) ) ;
#6224 = ORIENTED_EDGE ( 'NONE', *, *, #17736, .F. ) ;
#6225 = VERTEX_POINT ( 'NONE', #7647 ) ;
#6226 = EDGE_CURVE ( 'NONE', #3988, #6455, #10898, .T. ) ;
#6227 = LINE ( 'NONE', #9178, #13878 ) ;
#6228 = CARTESIAN_POINT ( 'NONE',  ( 32.50000000000000000, -21.50000000000000000, 3.680389326632394941E-13 ) ) ;
#6229 =( GEOMETRIC_REPRESENTATION_CONTEXT ( 3 ) GLOBAL_UNCERTAINTY_ASSIGNED_CONTEXT ( ( #76 ) ) GLOBAL_UNIT_ASSIGNED_CONTEXT ( ( #4261, #8533, #16150 ) ) REPRESENTATION_CONTEXT ( 'NONE', 'WORKASPACE' ) );
#6230 = CARTESIAN_POINT ( 'NONE',  ( 10.00000000000000000, -16.10733642026445978, -53.89344778774828626 ) ) ;
#6231 = EDGE_LOOP ( 'NONE', ( #11120, #15451, #9633, #18703, #12842 ) ) ;
#6232 = CIRCLE ( 'NONE', #15673, 56.24900000005625600 ) ;
#6233 = CIRCLE ( 'NONE', #17780, 0.2500000000000002220 ) ;
#6234 = DIRECTION ( 'NONE',  ( -1.000000000000000000, -0.000000000000000000, -0.000000000000000000 ) ) ;
#6235 = DIRECTION ( 'NONE',  ( 0.03086419753086420623, -0.9995235871707959241, 0.000000000000000000 ) ) ;
#6236 = CARTESIAN_POINT ( 'NONE',  ( 6.735557395310442615E-15, 3.000000000000000000, 55.00000000000000000 ) ) ;
#6237 = VERTEX_POINT ( 'NONE', #17842 ) ;
#6238 = DIRECTION ( 'NONE',  ( -1.000000000000000000, 0.000000000000000000, -0.000000000000000000 ) ) ;
#6239 = AXIS2_PLACEMENT_3D ( 'NONE', #1088, #5478, #2320 ) ;
#6240 = CIRCLE ( 'NONE', #1384, 63.00000000006298961 ) ;
#6241 = VERTEX_POINT ( 'NONE', #13186 ) ;
#6242 = DIRECTION ( 'NONE',  ( 0.000000000000000000, 0.000000000000000000, 1.000000000000000000 ) ) ;
#6243 = AXIS2_PLACEMENT_3D ( 'NONE', #15463, #18118, #6702 ) ;
#6244 = ORIENTED_EDGE ( 'NONE', *, *, #8492, .T. ) ;
#6245 = CARTESIAN_POINT ( 'NONE',  ( 32.50000000000000000, -34.99999999999999289, 3.680389326632394941E-13 ) ) ;
#6246 = CARTESIAN_POINT ( 'NONE',  ( -3.522875095019672109, 2.820352903225427532, -3.598441714920591394 ) ) ;
#6247 = ORIENTED_EDGE ( 'NONE', *, *, #5822, .T. ) ;
#6248 = ORIENTED_EDGE ( 'NONE', *, *, #6014, .T. ) ;
#6249 = EDGE_CURVE ( 'NONE', #17591, #4170, #5753, .T. ) ;
#6250 = CARTESIAN_POINT ( 'NONE',  ( 10.00000000000000000, -40.70683587897930522, -38.81885513160031564 ) ) ;
#6251 = VERTEX_POINT ( 'NONE', #8972 ) ;
#6252 = CYLINDRICAL_SURFACE ( 'NONE', #13989, 24.00000000002399858 ) ;
#6253 = AXIS2_PLACEMENT_3D ( 'NONE', #9396, #5201, #5393 ) ;
#6254 = CIRCLE ( 'NONE', #18107, 2.649999999999999467 ) ;
#6255 = CARTESIAN_POINT ( 'NONE',  ( 0.000000000000000000, -15.68049343255974826, -29.03656532225581088 ) ) ;
#6256 = ORIENTED_EDGE ( 'NONE', *, *, #8900, .F. ) ;
#6257 = ADVANCED_FACE ( 'NONE', ( #4696 ), #14901, .T. ) ;
#6258 = AXIS2_PLACEMENT_3D ( 'NONE', #6421, #7938, #8029 ) ;
#6259 = ORIENTED_EDGE ( 'NONE', *, *, #7196, .F. ) ;
#6260 = ADVANCED_BREP_SHAPE_REPRESENTATION ( '', ( #15847, #8017 ), #11074 ) ;
#6261 = CARTESIAN_POINT ( 'NONE',  ( 0.000000000000000000, 3.000000000000000000, 0.000000000000000000 ) ) ;
#6262 = DIRECTION ( 'NONE',  ( 0.000000000000000000, -1.224646799147353454E-16, 1.000000000000000000 ) ) ;
#6264 = AXIS2_PLACEMENT_3D ( 'NONE', #10502, #8804, #331 ) ;
#6263 = CARTESIAN_POINT ( 'NONE',  ( 0.000000000000000000, 0.000000000000000000, 0.000000000000000000 ) ) ;
#6265 = VERTEX_POINT ( 'NONE', #7560 ) ;
#6266 = CARTESIAN_POINT ( 'NONE',  ( 1.567478505476134803E-15, 4.618802153517012954, -3.504269196027872457 ) ) ;
#6267 = EDGE_CURVE ( 'NONE', #6186, #14980, #13382, .T. ) ;
#6268 = AXIS2_PLACEMENT_3D ( 'NONE', #6312, #9353, #16790 ) ;
#6269 = CARTESIAN_POINT ( 'NONE',  ( 0.000000000000000000, 0.000000000000000000, 0.000000000000000000 ) ) ;
#6270 = CARTESIAN_POINT ( 'NONE',  ( 10.00000000000000000, -55.83748330407413363, 7.813799127873079620 ) ) ;
#6271 = CIRCLE ( 'NONE', #17235, 24.00000000002400569 ) ;
#6272 = DIRECTION ( 'NONE',  ( 0.000000000000000000, 0.000000000000000000, -1.000000000000000000 ) ) ;
#6273 = ORIENTED_EDGE ( 'NONE', *, *, #9923, .F. ) ;
#6274 = CARTESIAN_POINT ( 'NONE',  ( 10.00000000000000000, 5.086963483077203918, 27.72801475327284138 ) ) ;
#6275 = AXIS2_PLACEMENT_3D ( 'NONE', #7895, #13711, #2091 ) ;
#6276 = VERTEX_POINT ( 'NONE', #16321 ) ;
#6277 = DIRECTION ( 'NONE',  ( 0.000000000000000000, 0.000000000000000000, 1.000000000000000000 ) ) ;
#6278 = DIRECTION ( 'NONE',  ( -0.000000000000000000, -1.000000000000000000, -0.000000000000000000 ) ) ;
#6279 = ADVANCED_FACE ( 'NONE', ( #6704 ), #6792, .T. ) ;
#6280 = AXIS2_PLACEMENT_3D ( 'NONE', #6477, #12477, #6571 ) ;
#6281 = AXIS2_PLACEMENT_3D ( 'NONE', #12875, #18673, #8663 ) ;
#6282 = AXIS2_PLACEMENT_3D ( 'NONE', #4952, #2280, #7998 ) ;
#6283 = AXIS2_PLACEMENT_3D ( 'NONE', #14783, #10595, #6121 ) ;
#6284 = AXIS2_PLACEMENT_3D ( 'NONE', #3918, #5039, #9616 ) ;
#6285 = ORIENTED_EDGE ( 'NONE', *, *, #2489, .T. ) ;
#6286 = FACE_OUTER_BOUND ( 'NONE', #540, .T. ) ;
#6287 = ORIENTED_EDGE ( 'NONE', *, *, #8988, .T. ) ;
#6288 = FILL_AREA_STYLE_COLOUR ( '', #14871 ) ;
#6289 = FACE_OUTER_BOUND ( 'NONE', #3099, .T. ) ;
#6290 = DIRECTION ( 'NONE',  ( -0.000000000000000000, 1.000000000000000000, -0.000000000000000000 ) ) ;
#6291 = LINE ( 'NONE', #6195, #17102 ) ;
#6292 = CIRCLE ( 'NONE', #8440, 24.00000000002399858 ) ;
#6293 = DIRECTION ( 'NONE',  ( -1.000000000000000000, -0.000000000000000000, 0.000000000000000000 ) ) ;
#6294 = ORIENTED_EDGE ( 'NONE', *, *, #14776, .T. ) ;
#6295 = DIRECTION ( 'NONE',  ( -1.000000000000000000, 0.000000000000000000, 0.000000000000000000 ) ) ;
#6296 = CIRCLE ( 'NONE', #7522, 56.24900000005625600 ) ;
#6297 = FACE_OUTER_BOUND ( 'NONE', #5457, .T. ) ;
#6298 = ORIENTED_EDGE ( 'NONE', *, *, #18060, .T. ) ;
#6299 = AXIS2_PLACEMENT_3D ( 'NONE', #6000, #17631, #2165 ) ;
#6300 = AXIS2_PLACEMENT_3D ( 'NONE', #12121, #12302, #14898 ) ;
#6301 = ORIENTED_EDGE ( 'NONE', *, *, #4286, .T. ) ;
#6302 = EDGE_CURVE ( 'NONE', #421, #10185, #9579, .T. ) ;
#6303 = EDGE_CURVE ( 'NONE', #16309, #9028, #3949, .T. ) ;
#6304 = VERTEX_POINT ( 'NONE', #15354 ) ;
#6305 = AXIS2_PLACEMENT_3D ( 'NONE', #3506, #9127, #16267 ) ;
#6306 = ORIENTED_EDGE ( 'NONE', *, *, #13437, .T. ) ;
#6307 = AXIS2_PLACEMENT_3D ( 'NONE', #4797, #12028, #6223 ) ;
#6308 = DIRECTION ( 'NONE',  ( 0.000000000000000000, -0.000000000000000000, -1.000000000000000000 ) ) ;
#6309 = DIRECTION ( 'NONE',  ( -0.000000000000000000, -1.000000000000000000, -0.000000000000000000 ) ) ;
#6310 = VECTOR ( 'NONE', #12430, 1000.000000000000000 ) ;
#6311 = DIRECTION ( 'NONE',  ( 0.000000000000000000, -1.000000000000000000, -1.047444401652940007E-14 ) ) ;
#6312 = CARTESIAN_POINT ( 'NONE',  ( 2.500000000000000000, 2.357898499370431722, -2.818925648462311528E-15 ) ) ;
#6313 = EDGE_CURVE ( 'NONE', #6177, #12431, #16997, .T. ) ;
#6314 = DIRECTION ( 'NONE',  ( 0.000000000000000000, 0.000000000000000000, -1.000000000000000000 ) ) ;
#6315 = FACE_OUTER_BOUND ( 'NONE', #17992, .T. ) ;
#6316 = CARTESIAN_POINT ( 'NONE',  ( 5.000000000000000000, -29.75305054077482936, 14.27431201565513774 ) ) ;
#6317 = CARTESIAN_POINT ( 'NONE',  ( 10.00000000000000000, 0.000000000000000000, 0.000000000000000000 ) ) ;
#6318 = ORIENTED_EDGE ( 'NONE', *, *, #13646, .F. ) ;
#6319 = FACE_OUTER_BOUND ( 'NONE', #13161, .T. ) ;
#6320 = ORIENTED_EDGE ( 'NONE', *, *, #17413, .F. ) ;
#6321 = DIRECTION ( 'NONE',  ( 0.000000000000000000, 0.000000000000000000, 1.000000000000000000 ) ) ;
#6322 = EDGE_CURVE ( 'NONE', #7275, #10830, #5125, .T. ) ;
#6323 = CARTESIAN_POINT ( 'NONE',  ( 3.861362476283255685, 2.629030857715988656, -3.671615880910370500 ) ) ;
#6324 = DIRECTION ( 'NONE',  ( -1.000000000000000000, 0.000000000000000000, 0.000000000000000000 ) ) ;
#6325 = CIRCLE ( 'NONE', #5403, 0.09999999999999939493 ) ;
#6326 = ORIENTED_EDGE ( 'NONE', *, *, #12052, .F. ) ;
#6327 = EDGE_LOOP ( 'NONE', ( #13120, #2232, #4827, #6580 ) ) ;
#6328 = CARTESIAN_POINT ( 'NONE',  ( -11.15000000000000391, 0.000000000000000000, 0.000000000000000000 ) ) ;
#6329 = DIRECTION ( 'NONE',  ( 0.000000000000000000, 0.000000000000000000, 1.000000000000000000 ) ) ;
#6330 = AXIS2_PLACEMENT_3D ( 'NONE', #17816, #14883, #10315 ) ;
#6331 = CARTESIAN_POINT ( 'NONE',  ( 4.799999999999999822, 0.000000000000000000, -1.000000000000000000 ) ) ;
#6332 = ORIENTED_EDGE ( 'NONE', *, *, #10747, .T. ) ;
#6333 = CIRCLE ( 'NONE', #5433, 12.00000000001200462 ) ;
#6334 = CIRCLE ( 'NONE', #14863, 24.00000000002399858 ) ;
#6335 = EDGE_CURVE ( 'NONE', #1805, #6013, #7557, .T. ) ;
#6336 = ADVANCED_FACE ( 'NONE', ( #18120 ), #2037, .T. ) ;
#6337 = PRODUCT ( 'Indexing Ring', 'Indexing Ring', '', ( #10128 ) ) ;
#6338 = CARTESIAN_POINT ( 'NONE',  ( -8.060728450267886203, -24.77235419320996002, -2.000000000000000000 ) ) ;
#6339 = EDGE_CURVE ( 'NONE', #5103, #13033, #3746, .T. ) ;
#6340 = FACE_BOUND ( 'NONE', #7111, .T. ) ;
#6341 = AXIS2_PLACEMENT_3D ( 'NONE', #633, #17589, #3206 ) ;
#6342 = CARTESIAN_POINT ( 'NONE',  ( 0.000000000000000000, 26.45033635316149301, 33.75576474687247241 ) ) ;
#6343 = ADVANCED_FACE ( 'NONE', ( #12507, #7840 ), #10880, .F. ) ;
#6344 = ORIENTED_EDGE ( 'NONE', *, *, #16340, .F. ) ;
#6345 = DIRECTION ( 'NONE',  ( 0.000000000000000000, 0.000000000000000000, -1.000000000000000000 ) ) ;
#6346 = AXIS2_PLACEMENT_3D ( 'NONE', #10563, #17710, #6277 ) ;
#6347 = AXIS2_PLACEMENT_3D ( 'NONE', #5253, #9537, #15551 ) ;
#6348 = VERTEX_POINT ( 'NONE', #2416 ) ;
#6349 = AXIS2_PLACEMENT_3D ( 'NONE', #9504, #10826, #5016 ) ;
#6350 = DIRECTION ( 'NONE',  ( 0.000000000000000000, 0.000000000000000000, 1.000000000000000000 ) ) ;
#6351 = ORIENTED_EDGE ( 'NONE', *, *, #17601, .T. ) ;
#6352 = CARTESIAN_POINT ( 'NONE',  ( 10.00000000000000000, -56.37237871411034718, 1.017308535512174261 ) ) ;
#6353 = DIRECTION ( 'NONE',  ( 1.000000000000000000, 0.000000000000000000, 0.000000000000000000 ) ) ;
#6354 = VERTEX_POINT ( 'NONE', #13660 ) ;
#6355 = ORIENTED_EDGE ( 'NONE', *, *, #6643, .T. ) ;
#6356 = DIRECTION ( 'NONE',  ( 0.000000000000000000, 0.000000000000000000, 1.000000000000000000 ) ) ;
#6357 = ORIENTED_EDGE ( 'NONE', *, *, #6894, .T. ) ;
#6358 = CARTESIAN_POINT ( 'NONE',  ( 6.080745460913608902, 0.5192545390863916310, -1.000000000000000000 ) ) ;
#6359 = AXIS2_PLACEMENT_3D ( 'NONE', #8802, #5488, #15365 ) ;
#6360 = VECTOR ( 'NONE', #11968, 1000.000000000000000 ) ;
#6361=STYLED_ITEM('',(#18890),#15935);
#6362 = AXIS2_PLACEMENT_3D ( 'NONE', #18734, #4276, #13125 ) ;
#6363 = PLANE ( 'NONE',  #16880 ) ;
#6364 = ADVANCED_FACE ( 'NONE', ( #608 ), #702, .T. ) ;
#6365 = ORIENTED_EDGE ( 'NONE', *, *, #10984, .T. ) ;
#6366 = AXIS2_PLACEMENT_3D ( 'NONE', #6110, #7539, #13361 ) ;
#6367 = ORIENTED_EDGE ( 'NONE', *, *, #14132, .T. ) ;
#6368 = FACE_OUTER_BOUND ( 'NONE', #12317, .T. ) ;
#6369 = DIRECTION ( 'NONE',  ( -1.000000000000000000, 0.000000000000000000, -0.000000000000000000 ) ) ;
#6370 = CARTESIAN_POINT ( 'NONE',  ( 0.000000000000000000, 1.305124410222461284, -2.000000000000000000 ) ) ;
#6371 = ORIENTED_EDGE ( 'NONE', *, *, #4637, .T. ) ;
#6372 = DIRECTION ( 'NONE',  ( -1.000000000000000000, 0.000000000000000000, 0.000000000000000000 ) ) ;
#6373 = CIRCLE ( 'NONE', #17032, 5.000000000000004441 ) ;
#6374 = CARTESIAN_POINT ( 'NONE',  ( -117.1020693116508085, -34.99999999999999289, 19.69080595179778115 ) ) ;
#6375 = DIRECTION ( 'NONE',  ( 0.000000000000000000, 0.000000000000000000, 1.000000000000000000 ) ) ;
#6376 = CARTESIAN_POINT ( 'NONE',  ( -11.25000000000000355, 0.000000000000000000, 0.000000000000000000 ) ) ;
#6377 = VERTEX_POINT ( 'NONE', #4974 ) ;
#6378 = PRESENTATION_STYLE_ASSIGNMENT (( #1808 ) ) ;
#6379 = EDGE_LOOP ( 'NONE', ( #7991, #10078, #2992, #10698 ) ) ;
#6380 = LINE ( 'NONE', #15145, #7282 ) ;
#6381 = CARTESIAN_POINT ( 'NONE',  ( 10.00000000000000000, -7.813799127873676476, 55.83748330407405547 ) ) ;
#6382 = CIRCLE ( 'NONE', #15809, 24.00000000002399858 ) ;
#6383 = AXIS2_PLACEMENT_3D ( 'NONE', #15855, #15765, #1198 ) ;
#6384 = EDGE_CURVE ( 'NONE', #9892, #3169, #5260, .T. ) ;
#6385 = ORIENTED_EDGE ( 'NONE', *, *, #17962, .T. ) ;
#6386 = VERTEX_POINT ( 'NONE', #2308 ) ;
#6387 = CARTESIAN_POINT ( 'NONE',  ( 4.000000000000000000, 1.680228229147133767, -3.316631783032546021 ) ) ;
#6388 = DIRECTION ( 'NONE',  ( 0.000000000000000000, 0.5000000000000011102, 0.8660254037844380415 ) ) ;
#6389 = CARTESIAN_POINT ( 'NONE',  ( 32.50000000000000000, -30.00000000000000000, 3.680389326632394941E-13 ) ) ;
#6390 = FACE_OUTER_BOUND ( 'NONE', #17351, .T. ) ;
#6391 = CARTESIAN_POINT ( 'NONE',  ( -1.200950573245989306, 13.24999999999999822, 24.97113769375797432 ) ) ;
#6392 = ORIENTED_EDGE ( 'NONE', *, *, #7018, .F. ) ;
#6394 = DIRECTION ( 'NONE',  ( 0.000000000000000000, 0.000000000000000000, 1.000000000000000000 ) ) ;
#6393 = CIRCLE ( 'NONE', #17058, 0.09999999999999939493 ) ;
#6395 = MECHANICAL_DESIGN_GEOMETRIC_PRESENTATION_REPRESENTATION (  '', ( #16446 ), #8532 ) ;
#6396 =( NAMED_UNIT ( * ) SI_UNIT ( $, .STERADIAN. ) SOLID_ANGLE_UNIT ( ) );
#6397 = LINE ( 'NONE', #16580, #5432 ) ;
#6398 = ORIENTED_EDGE ( 'NONE', *, *, #235, .T. ) ;
#6399 = EDGE_CURVE ( 'NONE', #4564, #18729, #2399, .T. ) ;
#6400 = CONTEXT_DEPENDENT_SHAPE_REPRESENTATION ( #10712, #13639 ) ;
#6401 = ORIENTED_EDGE ( 'NONE', *, *, #9226, .T. ) ;
#6402 = ADVANCED_FACE ( 'NONE', ( #3567 ), #9360, .T. ) ;
#6403 = ORIENTED_EDGE ( 'NONE', *, *, #3824, .F. ) ;
#6404 = VERTEX_POINT ( 'NONE', #2127 ) ;
#6405 = DIRECTION ( 'NONE',  ( -1.000000000000000000, -0.000000000000000000, -0.000000000000000000 ) ) ;
#6406 = DIRECTION ( 'NONE',  ( 1.000000000000000000, 0.000000000000000000, 0.000000000000000000 ) ) ;
#6407 = CARTESIAN_POINT ( 'NONE',  ( 10.00000000000000000, 0.000000000000000000, 0.000000000000000000 ) ) ;
#6408 = CARTESIAN_POINT ( 'NONE',  ( 10.00000000000000000, 0.000000000000000000, 0.000000000000000000 ) ) ;
#6409 = CARTESIAN_POINT ( 'NONE',  ( 10.00000000000000000, -15.68049343256016570, 29.03656532225557996 ) ) ;
#6410 = CARTESIAN_POINT ( 'NONE',  ( 10.00000000000000000, -56.23315539212691050, 1.335003989221430487 ) ) ;
#6411 = DIRECTION ( 'NONE',  ( -1.000000000000000000, 0.000000000000000000, 0.000000000000000000 ) ) ;
#6412 = CARTESIAN_POINT ( 'NONE',  ( -290.0000000000001705, -30.00000000000000000, 125.0000000000000000 ) ) ;
#6413 = ORIENTED_EDGE ( 'NONE', *, *, #6399, .T. ) ;
#6414 = DIRECTION ( 'NONE',  ( -1.000000000000000000, 0.000000000000000000, 0.000000000000000000 ) ) ;
#6415 = ORIENTED_EDGE ( 'NONE', *, *, #12557, .T. ) ;
#6416 = DIRECTION ( 'NONE',  ( -1.000000000000000000, -0.000000000000000000, -0.000000000000000000 ) ) ;
#6417 = CARTESIAN_POINT ( 'NONE',  ( 13.90576474687263264, 10.00000000000000000, -45.44754323328189827 ) ) ;
#6418 = CARTESIAN_POINT ( 'NONE',  ( 10.00000000000000000, 0.000000000000000000, 0.000000000000000000 ) ) ;
#6419 = VERTEX_POINT ( 'NONE', #7931 ) ;
#6420 = VERTEX_POINT ( 'NONE', #18312 ) ;
#6421 = CARTESIAN_POINT ( 'NONE',  ( -26.29305231718568336, -26.50000000000000000, -19.10302069950552095 ) ) ;
#6422 = AXIS2_PLACEMENT_3D ( 'NONE', #13352, #6100, #2783 ) ;
#6423 = CARTESIAN_POINT ( 'NONE',  ( 3.851859888774471706E-31, -1.249999999999999334, 0.000000000000000000 ) ) ;
#6424 = DIRECTION ( 'NONE',  ( 0.000000000000000000, 0.000000000000000000, 1.000000000000000000 ) ) ;
#6425 = ORIENTED_EDGE ( 'NONE', *, *, #11490, .T. ) ;
#6426 = EDGE_CURVE ( 'NONE', #9272, #10759, #7860, .T. ) ;
#6427 = DIRECTION ( 'NONE',  ( 0.000000000000000000, 0.000000000000000000, 1.000000000000000000 ) ) ;
#6428 = CARTESIAN_POINT ( 'NONE',  ( 2.500000000000000000, 2.500728763858895382E-16, -2.041999999999999815 ) ) ;
#6429 = CYLINDRICAL_SURFACE ( 'NONE', #16975, 56.24900000005625600 ) ;
#6430 = ORIENTED_EDGE ( 'NONE', *, *, #15174, .T. ) ;
#6432 = VECTOR ( 'NONE', #14818, 1000.000000000000000 ) ;
#6431 = CARTESIAN_POINT ( 'NONE',  ( 10.00000000000000000, -18.38754094778203552, -53.29895248911694239 ) ) ;
#6433 = CIRCLE ( 'NONE', #3713, 2.055000000000000160 ) ;
#6434 = VERTEX_POINT ( 'NONE', #6606 ) ;
#6435 = CYLINDRICAL_SURFACE ( 'NONE', #1752, 2.500000000000000444 ) ;
#6436 = VERTEX_POINT ( 'NONE', #18224 ) ;
#6437 = EDGE_CURVE ( 'NONE', #7035, #12068, #10973, .T. ) ;
#6438 = EDGE_CURVE ( 'NONE', #12051, #8217, #10030, .T. ) ;
#6439 = CIRCLE ( 'NONE', #16479, 2.499999999999999556 ) ;
#6440 = EDGE_CURVE ( 'NONE', #7515, #12362, #6658, .T. ) ;
#6441 = LINE ( 'NONE', #16914, #1712 ) ;
#6442 = CARTESIAN_POINT ( 'NONE',  ( -2.712762565639006418, 3.052587955997511759, -3.430618716626627318 ) ) ;
#6443 = EDGE_LOOP ( 'NONE', ( #15003, #15920, #12938, #14545 ) ) ;
#6444 = ORIENTED_EDGE ( 'NONE', *, *, #465, .F. ) ;
#6445 = CARTESIAN_POINT ( 'NONE',  ( -56.50000000009000445, -30.00000000000000000, 3.817814120399276590E-13 ) ) ;
#6446 = EDGE_CURVE ( 'NONE', #13569, #6386, #9077, .T. ) ;
#6447 = ORIENTED_EDGE ( 'NONE', *, *, #16221, .T. ) ;
#6448 = PLANE ( 'NONE',  #13676 ) ;
#6449 = ADVANCED_FACE ( 'NONE', ( #8685 ), #35, .T. ) ;
#6450 = EDGE_CURVE ( 'NONE', #514, #10074, #10600, .T. ) ;
#6451 = AXIS2_PLACEMENT_3D ( 'NONE', #5810, #4380, #17518 ) ;
#6452 = DIRECTION ( 'NONE',  ( 0.000000000000000000, 0.000000000000000000, 1.000000000000000000 ) ) ;
#6453 = DIRECTION ( 'NONE',  ( 0.000000000000000000, 0.000000000000000000, 1.000000000000000000 ) ) ;
#6454 = ORIENTED_EDGE ( 'NONE', *, *, #14959, .F. ) ;
#6455 = VERTEX_POINT ( 'NONE', #17370 ) ;
#6456 = CARTESIAN_POINT ( 'NONE',  ( 10.00000000000000000, -50.69000562871659810, 24.68609584167141691 ) ) ;
#6457 = CARTESIAN_POINT ( 'NONE',  ( 10.00000000000000000, -14.27431201565546104, 29.75305054077466949 ) ) ;
#6458 = DIRECTION ( 'NONE',  ( -1.000000000000000000, -0.000000000000000000, 0.000000000000000000 ) ) ;
#6459 = ORIENTED_EDGE ( 'NONE', *, *, #10636, .F. ) ;
#6460 = CARTESIAN_POINT ( 'NONE',  ( -117.1020693116508085, -38.00000000000000000, 19.69080595179778115 ) ) ;
#6461 = EDGE_CURVE ( 'NONE', #7707, #2698, #15497, .T. ) ;
#6462 = DIRECTION ( 'NONE',  ( -1.000000000000000000, 0.000000000000000000, 0.000000000000000000 ) ) ;
#6463 = FACE_OUTER_BOUND ( 'NONE', #8475, .T. ) ;
#6464 = CARTESIAN_POINT ( 'NONE',  ( 4.197393957002303999, 0.8151795401431359833, -3.503767560748935139 ) ) ;
#6465 = ORIENTED_EDGE ( 'NONE', *, *, #6596, .F. ) ;
#6466 = CARTESIAN_POINT ( 'NONE',  ( -117.1020693116506379, -30.00000000000000000, -17.04080595179802415 ) ) ;
#6467 = VECTOR ( 'NONE', #14946, 1000.000000000000000 ) ;
#6468 = ORIENTED_EDGE ( 'NONE', *, *, #6335, .T. ) ;
#6469 = CARTESIAN_POINT ( 'NONE',  ( 11.24999999999999645, 0.000000000000000000, 0.000000000000000000 ) ) ;
#6470 = AXIS2_PLACEMENT_3D ( 'NONE', #12215, #3371, #18024 ) ;
#6471 = DIRECTION ( 'NONE',  ( -1.000000000000000000, 0.000000000000000000, 0.000000000000000000 ) ) ;
#6472 =( REPRESENTATION_RELATIONSHIP ('NONE','NONE', #11014, #16742 ) REPRESENTATION_RELATIONSHIP_WITH_TRANSFORMATION ( #7165 )SHAPE_REPRESENTATION_RELATIONSHIP( ) );
#6473 = EDGE_CURVE ( 'NONE', #364, #15019, #7278, .T. ) ;
#6474 = ORIENTED_EDGE ( 'NONE', *, *, #7486, .T. ) ;
#6475 = CIRCLE ( 'NONE', #17732, 33.00000000003299760 ) ;
#6476 = ORIENTED_EDGE ( 'NONE', *, *, #8643, .F. ) ;
#6477 = CARTESIAN_POINT ( 'NONE',  ( 10.00000000000000000, 45.00825343885021113, 33.95787273855260935 ) ) ;
#6478 = CIRCLE ( 'NONE', #9514, 2.649999999999985700 ) ;
#6479 = DIRECTION ( 'NONE',  ( 0.000000000000000000, 1.000000000000000000, 0.000000000000000000 ) ) ;
#6480 = DIRECTION ( 'NONE',  ( 0.000000000000000000, 0.000000000000000000, -1.000000000000000000 ) ) ;
#6481 = CARTESIAN_POINT ( 'NONE',  ( 10.00000000000000000, -33.71303790549312396, 53.22058882792185130 ) ) ;
#6482 = DIRECTION ( 'NONE',  ( -1.000000000000000000, -0.000000000000000000, 0.000000000000000000 ) ) ;
#6483 = CYLINDRICAL_SURFACE ( 'NONE', #17523, 24.00000000002399858 ) ;
#6484 = ORIENTED_EDGE ( 'NONE', *, *, #41, .T. ) ;
#6485 = DIRECTION ( 'NONE',  ( 0.000000000000000000, 0.000000000000000000, 1.000000000000000000 ) ) ;
#6486 = DIRECTION ( 'NONE',  ( -0.9396926207859138680, 0.000000000000000000, -0.3420201433256536139 ) ) ;
#6487 = EDGE_LOOP ( 'NONE', ( #437, #10403, #3950, #11404 ) ) ;
#6488 = EDGE_CURVE ( 'NONE', #8855, #2916, #11235, .T. ) ;
#6489 = ITEM_DEFINED_TRANSFORMATION ( 'NONE', 'NONE', #8960,  #8017 ) ;
#6490 = VECTOR ( 'NONE', #2508, 1000.000000000000000 ) ;
#6491 = ORIENTED_EDGE ( 'NONE', *, *, #15039, .T. ) ;
#6492 = ORIENTED_EDGE ( 'NONE', *, *, #7937, .T. ) ;
#6493 = ORIENTED_EDGE ( 'NONE', *, *, #2311, .F. ) ;
#6494 = DIRECTION ( 'NONE',  ( -1.000000000000000000, 0.000000000000000000, 0.000000000000000000 ) ) ;
#6495 = CARTESIAN_POINT ( 'NONE',  ( 2.500000000000000000, 0.000000000000000000, 0.000000000000000000 ) ) ;
#6496 = DIRECTION ( 'NONE',  ( 1.000000000000000000, 0.000000000000000000, 0.000000000000000000 ) ) ;
#6497 = DIRECTION ( 'NONE',  ( 0.000000000000000000, -0.1564344650402171299, -0.9876883405951398798 ) ) ;
#6498 = AXIS2_PLACEMENT_3D ( 'NONE', #7349, #13171, #8509 ) ;
#6499 = ADVANCED_FACE ( 'NONE', ( #2791 ), #15929, .T. ) ;
#6500 = FACE_BOUND ( 'NONE', #1449, .T. ) ;
#6501 = DIRECTION ( 'NONE',  ( -1.000000000000000000, -0.000000000000000000, 0.000000000000000000 ) ) ;
#6502 = PLANE ( 'NONE',  #12637 ) ;
#6503 = EDGE_LOOP ( 'NONE', ( #17420, #2453, #1809, #6679 ) ) ;
#6504 = CARTESIAN_POINT ( 'NONE',  ( 0.000000000000000000, 15.00000000000000000, 0.000000000000000000 ) ) ;
#6505 = ORIENTED_EDGE ( 'NONE', *, *, #15300, .T. ) ;
#6506 = ADVANCED_FACE ( 'NONE', ( #14494 ), #11270, .F. ) ;
#6507 = LINE ( 'NONE', #15560, #16846 ) ;
#6508 = CARTESIAN_POINT ( 'NONE',  ( 10.00000000000000000, 34.13306034420185853, 44.70888270294173594 ) ) ;
#6509 = VERTEX_POINT ( 'NONE', #5559 ) ;
#6510 = EDGE_LOOP ( 'NONE', ( #6318, #17787, #10513, #1301 ) ) ;
#6511 = CARTESIAN_POINT ( 'NONE',  ( -2.344047193898593395, -3.265465875126480455, -1.054683074273691752E-14 ) ) ;
#6512 = DIRECTION ( 'NONE',  ( -0.9873298794253687616, 1.799126239882928354E-16, 0.1586811557617578694 ) ) ;
#6513 = CARTESIAN_POINT ( 'NONE',  ( 0.000000000000000000, 0.000000000000000000, -5.000000000000000888 ) ) ;
#6514 = EDGE_LOOP ( 'NONE', ( #6415, #3313 ) ) ;
#6515 = PRESENTATION_LAYER_ASSIGNMENT (  '', '', ( #14130 ) ) ;
#6516 = CARTESIAN_POINT ( 'NONE',  ( 0.000000000000000000, 10.00000000000000000, 0.000000000000000000 ) ) ;
#6517 = CARTESIAN_POINT ( 'NONE',  ( 0.000000000000000000, -30.00000000000000000, 0.000000000000000000 ) ) ;
#6518 = CYLINDRICAL_SURFACE ( 'NONE', #5086, 63.00000000006298961 ) ;
#6519 = ORIENTED_EDGE ( 'NONE', *, *, #17359, .F. ) ;
#6520 = CARTESIAN_POINT ( 'NONE',  ( 10.00000000000000000, 0.000000000000000000, 0.000000000000000000 ) ) ;
#6521 = VERTEX_POINT ( 'NONE', #7261 ) ;
#6522 = UNCERTAINTY_MEASURE_WITH_UNIT (LENGTH_MEASURE( 1.000000000000000082E-05 ), #17644, 'distance_accuracy_value', 'NONE');
#6523 = DIRECTION ( 'NONE',  ( 0.000000000000000000, -0.5877852522924622569, -0.8090169943749552228 ) ) ;
#6524 = ORIENTED_EDGE ( 'NONE', *, *, #13090, .T. ) ;
#6525 = AXIS2_PLACEMENT_3D ( 'NONE', #1658, #11672, #241 ) ;
#6526 = DIRECTION ( 'NONE',  ( 0.000000000000000000, 0.000000000000000000, 1.000000000000000000 ) ) ;
#6527 = CARTESIAN_POINT ( 'NONE',  ( 10.04305231718579705, -30.00000000000000000, 33.55933677959249195 ) ) ;
#6528 = ORIENTED_EDGE ( 'NONE', *, *, #8550, .T. ) ;
#6529 = ORIENTED_EDGE ( 'NONE', *, *, #6014, .F. ) ;
#6530 = DIRECTION ( 'NONE',  ( -0.000000000000000000, -1.000000000000000000, -0.000000000000000000 ) ) ;
#6531 = SURFACE_STYLE_USAGE ( .BOTH. , #16360 ) ;
#6532 = ORIENTED_EDGE ( 'NONE', *, *, #1461, .T. ) ;
#6533 = DIRECTION ( 'NONE',  ( -0.8660254037844373753, 0.5000000000000021094, 0.000000000000000000 ) ) ;
#6534 = EDGE_CURVE ( 'NONE', #12930, #353, #4247, .T. ) ;
#6535 = CARTESIAN_POINT ( 'NONE',  ( 0.000000000000000000, -1.178949249685214307, 2.042000000000001592 ) ) ;
#6536 = DIRECTION ( 'NONE',  ( 1.000000000000000000, 0.000000000000000000, 0.000000000000000000 ) ) ;
#6537 = ADVANCED_FACE ( 'NONE', ( #5646 ), #12895, .F. ) ;
#6538 = VECTOR ( 'NONE', #7577, 1000.000000000000000 ) ;
#6540 = CIRCLE ( 'NONE', #779, 2.649999999999999467 ) ;
#6539 = LINE ( 'NONE', #14582, #219 ) ;
#6541 = ORIENTED_EDGE ( 'NONE', *, *, #14187, .T. ) ;
#6542 = EDGE_CURVE ( 'NONE', #2260, #17356, #15748, .T. ) ;
#6543 = ORIENTED_EDGE ( 'NONE', *, *, #7593, .F. ) ;
#6544 = CARTESIAN_POINT ( 'NONE',  ( -79.64793068852927149, -30.00000000000000000, 34.51039329588763849 ) ) ;
#6545 = DIRECTION ( 'NONE',  ( 1.000000000000000000, 0.000000000000000000, -0.000000000000000000 ) ) ;
#6546 = DIRECTION ( 'NONE',  ( 0.000000000000000000, 0.000000000000000000, 1.000000000000000000 ) ) ;
#6547 = ORIENTED_EDGE ( 'NONE', *, *, #3670, .F. ) ;
#6548 = CARTESIAN_POINT ( 'NONE',  ( -117.1020693116506379, -34.99999999999999289, -22.34080595179800355 ) ) ;
#6549 = EDGE_CURVE ( 'NONE', #5078, #16102, #472, .T. ) ;
#6550 = DIRECTION ( 'NONE',  ( 0.000000000000000000, 0.5877852522924742473, -0.8090169943749465631 ) ) ;
#6551 = CARTESIAN_POINT ( 'NONE',  ( 0.000000000000000000, 0.5192545390863916310, -1.000000000000000000 ) ) ;
#6552 = AXIS2_PLACEMENT_3D ( 'NONE', #7313, #4186, #8640 ) ;
#6553 = ORIENTED_EDGE ( 'NONE', *, *, #14839, .T. ) ;
#6554 = DIRECTION ( 'NONE',  ( 0.000000000000000000, 0.000000000000000000, -1.000000000000000000 ) ) ;
#6555 = VERTEX_POINT ( 'NONE', #17280 ) ;
#6556 = CARTESIAN_POINT ( 'NONE',  ( 10.00000000000000000, 26.45033635316149301, 39.05576474687247668 ) ) ;
#6558 = EDGE_CURVE ( 'NONE', #2490, #432, #7160, .T. ) ;
#6557 = VERTEX_POINT ( 'NONE', #4229 ) ;
#6559 = DIRECTION ( 'NONE',  ( -1.000000000000000000, 0.000000000000000000, -0.000000000000000000 ) ) ;
#6560 = CARTESIAN_POINT ( 'NONE',  ( -0.2500000000000000000, -8.096141056083446585, -1.000000000000000000 ) ) ;
#6561 = AXIS2_PLACEMENT_3D ( 'NONE', #8719, #4534, #2634 ) ;
#6562 = VECTOR ( 'NONE', #16489, 1000.000000000000000 ) ;
#6563 = EDGE_CURVE ( 'NONE', #17369, #12910, #4501, .T. ) ;
#6564 = ADVANCED_FACE ( 'NONE', ( #14971 ), #8783, .F. ) ;
#6565 = AXIS2_PLACEMENT_3D ( 'NONE', #18433, #13776, #735 ) ;
#6566 = VECTOR ( 'NONE', #16425, 1000.000000000000000 ) ;
#6567 = VERTEX_POINT ( 'NONE', #13538 ) ;
#6568 = EDGE_CURVE ( 'NONE', #11810, #13117, #14880, .T. ) ;
#6569 = CIRCLE ( 'NONE', #14181, 12.00000000001200462 ) ;
#6570 = EDGE_LOOP ( 'NONE', ( #18716, #17875, #11757, #17064 ) ) ;
#6571 = DIRECTION ( 'NONE',  ( 0.000000000000000000, 0.8910065241883690090, -0.4539904997395448616 ) ) ;
#6572 = CIRCLE ( 'NONE', #8994, 2.649999999999999467 ) ;
#6573 = CARTESIAN_POINT ( 'NONE',  ( 4.000000000000000888, -0.8578082829538523635, -3.433262215449808696 ) ) ;
#6574 = VECTOR ( 'NONE', #103, 1000.000000000000000 ) ;
#6576 = ADVANCED_FACE ( 'NONE', ( #16297 ), #7714, .T. ) ;
#6575 = DIRECTION ( 'NONE',  ( -1.000000000000000000, -0.000000000000000000, 0.000000000000000000 ) ) ;
#6577 = DIRECTION ( 'NONE',  ( -1.000000000000000000, 0.000000000000000000, -0.000000000000000000 ) ) ;
#6578 = CARTESIAN_POINT ( 'NONE',  ( 0.2500000000000002220, 0.000000000000000000, 0.000000000000000000 ) ) ;
#6579 = LINE ( 'NONE', #3355, #11745 ) ;
#6580 = ORIENTED_EDGE ( 'NONE', *, *, #13036, .T. ) ;
#6581 = CARTESIAN_POINT ( 'NONE',  ( 10.00000000000000000, -10.11537145609416122, 55.33199130079781014 ) ) ;
#6582 = CARTESIAN_POINT ( 'NONE',  ( -4.000000000000000000, 0.000000000000000000, 0.000000000000000000 ) ) ;
#6583 = VERTEX_POINT ( 'NONE', #1632 ) ;
#6584 = AXIS2_PLACEMENT_3D ( 'NONE', #6612, #2134, #15362 ) ;
#6585 = CIRCLE ( 'NONE', #491, 24.00000000002400213 ) ;
#6586 = VERTEX_POINT ( 'NONE', #17814 ) ;
#6587 = VECTOR ( 'NONE', #15638, 1000.000000000000000 ) ;
#6588 = AXIS2_PLACEMENT_3D ( 'NONE', #18699, #1193, #2190 ) ;
#6589 = ORIENTED_EDGE ( 'NONE', *, *, #13220, .F. ) ;
#6590 = EDGE_LOOP ( 'NONE', ( #422, #4425 ) ) ;
#6591 = CARTESIAN_POINT ( 'NONE',  ( 0.000000000000000000, -26.50000000000000000, 0.000000000000000000 ) ) ;
#6592 = DIRECTION ( 'NONE',  ( 0.000000000000000000, 0.000000000000000000, 1.000000000000000000 ) ) ;
#6593 = AXIS2_PLACEMENT_3D ( 'NONE', #17065, #9717, #8287 ) ;
#6594 = VECTOR ( 'NONE', #17688, 1000.000000000000000 ) ;
#6595 = DIRECTION ( 'NONE',  ( -1.000000000000000000, 0.000000000000000000, 0.000000000000000000 ) ) ;
#6596 = EDGE_CURVE ( 'NONE', #13370, #8889, #13452, .T. ) ;
#6597 = CYLINDRICAL_SURFACE ( 'NONE', #12972, 2.649999999999999467 ) ;
#6599 = LINE ( 'NONE', #18021, #15216 ) ;
#6598 = VECTOR ( 'NONE', #1999, 1000.000000000000000 ) ;
#6600 = DIRECTION ( 'NONE',  ( 0.000000000000000000, 0.000000000000000000, -1.000000000000000000 ) ) ;
#6601 = DIRECTION ( 'NONE',  ( 0.000000000000000000, 0.000000000000000000, 1.000000000000000000 ) ) ;
#6602 = CIRCLE ( 'NONE', #17261, 0.1000000000000028644 ) ;
#6603 = CARTESIAN_POINT ( 'NONE',  ( 0.000000000000000000, 18.38754094778314752, -53.29895248911656580 ) ) ;
#6604 = ORIENTED_EDGE ( 'NONE', *, *, #13437, .F. ) ;
#6605 = AXIS2_PLACEMENT_3D ( 'NONE', #3959, #2799, #1284 ) ;
#6606 = CARTESIAN_POINT ( 'NONE',  ( -4.078421086530219064, -3.990950201428956845, 0.000000000000000000 ) ) ;
#6607 = ORIENTED_EDGE ( 'NONE', *, *, #704, .F. ) ;
#6608 = DIRECTION ( 'NONE',  ( 0.000000000000000000, 0.000000000000000000, 1.000000000000000000 ) ) ;
#6609 = CARTESIAN_POINT ( 'NONE',  ( 0.000000000000000000, 13.24999999999999467, 0.000000000000000000 ) ) ;
#6610 = EDGE_LOOP ( 'NONE', ( #17338, #11011, #5934, #16175 ) ) ;
#6611 = EDGE_LOOP ( 'NONE', ( #12785, #14367, #13409, #2510 ) ) ;
#6612 = CARTESIAN_POINT ( 'NONE',  ( 2.500000000000000000, 2.357898499370432166, -2.385244779468109755E-15 ) ) ;
#6613 = DIRECTION ( 'NONE',  ( 7.719519468096791570E-17, -1.000000000000000000, -1.110223024625156540E-16 ) ) ;
#6614 = DIRECTION ( 'NONE',  ( -1.000000000000000000, 0.000000000000000000, 0.000000000000000000 ) ) ;
#6615 = EDGE_LOOP ( 'NONE', ( #1735, #4440, #3484, #10637 ) ) ;
#6616 = AXIS2_PLACEMENT_3D ( 'NONE', #17784, #4843, #10449 ) ;
#6617 = CIRCLE ( 'NONE', #18773, 56.24900000005625600 ) ;
#6618 = VECTOR ( 'NONE', #14346, 1000.000000000000000 ) ;
#6619 = AXIS2_PLACEMENT_3D ( 'NONE', #1840, #9257, #15079 ) ;
#6620 = ADVANCED_FACE ( 'NONE', ( #11915 ), #11833, .F. ) ;
#6621 = DIRECTION ( 'NONE',  ( 0.000000000000000000, 0.000000000000000000, 1.000000000000000000 ) ) ;
#6622 = FACE_BOUND ( 'NONE', #4764, .T. ) ;
#6623 = FACE_OUTER_BOUND ( 'NONE', #3608, .T. ) ;
#6624 = EDGE_LOOP ( 'NONE', ( #15615, #3356, #10401, #7936, #521, #9517, #7804, #10679, #16439, #13089, #838, #1713, #15289, #18026, #16806, #733, #15116, #10801, #4645, #13838, #5173, #11838, #5357, #3774, #8921, #17187, #6273, #2752, #16284, #14223, #7478, #8232, #7271, #6797, #8042, #13993, #8184, #8273, #17389, #3573, #4629, #2852, #15466, #17415, #7587, #14615, #18104, #5059, #18012, #15205, #12914, #16688, #15971, #7816, #14162, #6863, #14650, #7332, #2838, #15777, #4635, #7583, #145, #12751, #10303, #16778, #12377, #6116, #16209, #11735, #7567, #64, #3984, #18050, #14881, #17876, #8038, #10042, #6664, #12439, #11643, #11153, #7393, #9444, #8163, #16084, #7097, #11882, #10673, #14390, #442, #9479, #3734, #6972, #7825, #1549, #11716, #9964, #14772, #11168, #14278, #14525, #8775, #17040, #2147, #1705, #5610, #3972, #18099, #556, #2466, #10789, #14272, #2391, #5651, #10603, #16096, #10358, #5619, #11512, #6709, #6425, #13720, #13673, #757, #16181, #14246, #18638, #7032, #14819, #2035, #17202, #2227, #10535, #5907, #5778, #2684, #17383, #11107, #18342, #14141, #17806, #15814, #2078, #9534, #5990, #11976, #2796, #12656, #7095, #16483, #16827, #7306, #788, #16375, #569, #10991, #4701, #1986, #3502, #13506, #18671, #10070, #5218, #1573 ) ) ;
#6625 = CARTESIAN_POINT ( 'NONE',  ( 4.000000000000000000, -2.309401076758514915, -3.433295621305383349 ) ) ;
#6626 = AXIS2_PLACEMENT_3D ( 'NONE', #3987, #11218, #5212 ) ;
#6627 = EDGE_LOOP ( 'NONE', ( #10421, #15175, #11949, #7657, #9600, #2720, #6541, #7935, #4793, #10819, #5447, #13324 ) ) ;
#6628 = CARTESIAN_POINT ( 'NONE',  ( 2.500000000000000000, 0.000000000000000000, 0.000000000000000000 ) ) ;
#6629 = VERTEX_POINT ( 'NONE', #485 ) ;
#6630 = AXIS2_PLACEMENT_3D ( 'NONE', #7074, #10212, #5563 ) ;
#6631 = DIRECTION ( 'NONE',  ( 0.000000000000000000, 0.7071067811865486830, -0.7071067811865463515 ) ) ;
#6632 = CARTESIAN_POINT ( 'NONE',  ( 0.000000000000000000, 56.37237871411034007, 25.01730853553658207 ) ) ;
#6633 = CARTESIAN_POINT ( 'NONE',  ( 10.00000000000000000, 23.24033432160436874, 58.55669782892469755 ) ) ;
#6634 = CIRCLE ( 'NONE', #14536, 24.00000000002399858 ) ;
#6635 = VERTEX_POINT ( 'NONE', #1548 ) ;
#6636 = ORIENTED_EDGE ( 'NONE', *, *, #16162, .F. ) ;
#6637 = CIRCLE ( 'NONE', #17292, 24.00000000002399858 ) ;
#6638 = DIRECTION ( 'NONE',  ( 0.000000000000000000, -0.9510565162951565288, 0.3090169943749384029 ) ) ;
#6639 = ORIENTED_EDGE ( 'NONE', *, *, #14450, .T. ) ;
#6640 = LINE ( 'NONE', #551, #6067 ) ;
#6641 = EDGE_CURVE ( 'NONE', #4599, #2059, #2098, .T. ) ;
#6642 = VECTOR ( 'NONE', #2197, 1000.000000000000000 ) ;
#6643 = EDGE_CURVE ( 'NONE', #9892, #6992, #11836, .T. ) ;
#6644 = CYLINDRICAL_SURFACE ( 'NONE', #8693, 1.249999999999999778 ) ;
#6645 = COLOUR_RGB ( '',0.8941176470588234615, 0.8941176470588234615, 0.8941176470588234615 ) ;
#6646 = CIRCLE ( 'NONE', #10894, 56.24900000005625600 ) ;
#6647 = FACE_OUTER_BOUND ( 'NONE', #5346, .T. ) ;
#6648 = VERTEX_POINT ( 'NONE', #12105 ) ;
#6649 = ORIENTED_EDGE ( 'NONE', *, *, #15041, .T. ) ;
#6650 = LINE ( 'NONE', #11846, #17859 ) ;
#6651 = DIRECTION ( 'NONE',  ( 1.000000000000000000, 0.000000000000000000, 0.000000000000000000 ) ) ;
#6652 = LINE ( 'NONE', #13882, #16982 ) ;
#6653 = ORIENTED_EDGE ( 'NONE', *, *, #18788, .T. ) ;
#6654 = DIRECTION ( 'NONE',  ( 0.04803802292983955918, 0.000000000000000000, -0.9988455077503187729 ) ) ;
#6655 = ORIENTED_EDGE ( 'NONE', *, *, #12272, .F. ) ;
#6656 = CARTESIAN_POINT ( 'NONE',  ( 10.00000000000000000, -56.37237871411034718, 25.01730853553617351 ) ) ;
#6657 = DIRECTION ( 'NONE',  ( 1.000000000000000000, 0.000000000000000000, 0.000000000000000000 ) ) ;
#6658 = CIRCLE ( 'NONE', #12736, 0.7499999999999997780 ) ;
#6659 = ORIENTED_EDGE ( 'NONE', *, *, #6050, .F. ) ;
#6660 = ORIENTED_EDGE ( 'NONE', *, *, #507, .T. ) ;
#6661 = SURFACE_STYLE_FILL_AREA ( #860 ) ;
#6662 = AXIS2_PLACEMENT_3D ( 'NONE', #14100, #1166, #15631 ) ;
#6663 = ADVANCED_FACE ( 'NONE', ( #4400 ), #10476, .T. ) ;
#6664 = ORIENTED_EDGE ( 'NONE', *, *, #8367, .T. ) ;
#6665 = DIRECTION ( 'NONE',  ( 0.000000000000000000, 0.000000000000000000, 1.000000000000000000 ) ) ;
#6666 = DIRECTION ( 'NONE',  ( 1.000000000000000000, 0.000000000000000000, 0.000000000000000000 ) ) ;
#6667 = CIRCLE ( 'NONE', #10903, 63.00000000006298961 ) ;
#6668 = MECHANICAL_DESIGN_GEOMETRIC_PRESENTATION_REPRESENTATION (  '', ( #6361 ), #15787 ) ;
#6669 = CIRCLE ( 'NONE', #10593, 6.080745460913608902 ) ;
#6670 = VERTEX_POINT ( 'NONE', #7435 ) ;
#6671 = AXIS2_PLACEMENT_3D ( 'NONE', #12341, #3692, #3780 ) ;
#6672 = ORIENTED_EDGE ( 'NONE', *, *, #154, .T. ) ;
#6673 = LINE ( 'NONE', #14090, #17257 ) ;
#6674 = CARTESIAN_POINT ( 'NONE',  ( 10.00000000000000000, -54.20017844242489247, -32.11449294037253566 ) ) ;
#6675 = CARTESIAN_POINT ( 'NONE',  ( 10.00000000000000000, -34.13306034420153168, -44.70888270294199884 ) ) ;
#6676 = CYLINDRICAL_SURFACE ( 'NONE', #4179, 2.649999999999999467 ) ;
#6677 = DIRECTION ( 'NONE',  ( -0.000000000000000000, -0.000000000000000000, -1.000000000000000000 ) ) ;
#6678 = DIRECTION ( 'NONE',  ( -1.000000000000000000, 0.000000000000000000, -0.000000000000000000 ) ) ;
#6679 = ORIENTED_EDGE ( 'NONE', *, *, #1727, .T. ) ;
#6680 = EDGE_CURVE ( 'NONE', #14729, #12824, #6049, .T. ) ;
#6681 = ADVANCED_FACE ( 'NONE', ( #10312 ), #10582, .T. ) ;
#6682 = EDGE_CURVE ( 'NONE', #5250, #7010, #7630, .T. ) ;
#6683 = EDGE_CURVE ( 'NONE', #13795, #4644, #13255, .T. ) ;
#6684 = DIRECTION ( 'NONE',  ( 0.000000000000000000, 0.000000000000000000, -1.000000000000000000 ) ) ;
#6685 = AXIS2_PLACEMENT_3D ( 'NONE', #7330, #5901, #16098 ) ;
#6686 = DIRECTION ( 'NONE',  ( 1.000000000000000000, 0.000000000000000000, 0.000000000000000000 ) ) ;
#6687 = CONTEXT_DEPENDENT_SHAPE_REPRESENTATION ( #3188, #7378 ) ;
#6688 = COLOUR_RGB ( '',1.000000000000000000, 0.9490196078431372140, 0.9098039215686274384 ) ;
#6689 = EDGE_CURVE ( 'NONE', #14440, #10477, #16706, .T. ) ;
#6690 = ORIENTED_EDGE ( 'NONE', *, *, #341, .T. ) ;
#6691 = ORIENTED_EDGE ( 'NONE', *, *, #1291, .T. ) ;
#6692 = ORIENTED_EDGE ( 'NONE', *, *, #15995, .F. ) ;
#6693 = EDGE_CURVE ( 'NONE', #14039, #8760, #275, .T. ) ;
#6694 = CARTESIAN_POINT ( 'NONE',  ( 2.500000000000000000, -1.178949249685213863, 2.042000000000001148 ) ) ;
#6695 = CARTESIAN_POINT ( 'NONE',  ( 0.3865131578947368918, -23.49682122285426189, -2.000000000000000000 ) ) ;
#6696 = AXIS2_PLACEMENT_3D ( 'NONE', #2529, #15295, #8050 ) ;
#6697 = CARTESIAN_POINT ( 'NONE',  ( 0.000000000000000000, 0.000000000000000000, 0.000000000000000000 ) ) ;
#6698 = DIRECTION ( 'NONE',  ( -2.031314180040284764E-16, -1.000000000000000000, -1.301042606982601377E-16 ) ) ;
#6699 = CARTESIAN_POINT ( 'NONE',  ( 10.00000000000000000, -55.83748330407401284, -7.813799127873885197 ) ) ;
#6700 = DIRECTION ( 'NONE',  ( 0.000000000000000000, 0.000000000000000000, 1.000000000000000000 ) ) ;
#6701 = CARTESIAN_POINT ( 'NONE',  ( 0.000000000000000000, 0.000000000000000000, -30.00000000000000000 ) ) ;
#6702 = DIRECTION ( 'NONE',  ( 0.000000000000000000, 0.000000000000000000, 1.000000000000000000 ) ) ;
#6703 = EDGE_LOOP ( 'NONE', ( #13405, #7419, #1955, #3717 ) ) ;
#6704 = FACE_OUTER_BOUND ( 'NONE', #3390, .T. ) ;
#6705 = ORIENTED_EDGE ( 'NONE', *, *, #6917, .F. ) ;
#6706 = EDGE_CURVE ( 'NONE', #4819, #17330, #8797, .T. ) ;
#6707 = CARTESIAN_POINT ( 'NONE',  ( 0.000000000000000000, 46.20417134726132247, 32.31183295104789011 ) ) ;
#6708 = DIRECTION ( 'NONE',  ( 0.000000000000000000, 0.000000000000000000, 1.000000000000000000 ) ) ;
#6709 = ORIENTED_EDGE ( 'NONE', *, *, #11031, .F. ) ;
#6710 = ORIENTED_EDGE ( 'NONE', *, *, #8143, .T. ) ;
#6711 = CARTESIAN_POINT ( 'NONE',  ( 10.00000000000000000, 26.45033635316149301, 36.40576474687247099 ) ) ;
#6712 = CARTESIAN_POINT ( 'NONE',  ( -10.00000000000000000, 0.000000000000000000, 0.000000000000000000 ) ) ;
#6713 = ORIENTED_EDGE ( 'NONE', *, *, #220, .F. ) ;
#6714 = EDGE_CURVE ( 'NONE', #11663, #7605, #12755, .T. ) ;
#6715 = AXIS2_PLACEMENT_3D ( 'NONE', #16699, #9349, #17931 ) ;
#6716 = ADVANCED_FACE ( 'NONE', ( #10952 ), #4868, .T. ) ;
#6717 = LINE ( 'NONE', #14047, #7177 ) ;
#6718 = CARTESIAN_POINT ( 'NONE',  ( 0.000000000000000000, -47.29147401531984229, 41.62350880771904826 ) ) ;
#6719 = CARTESIAN_POINT ( 'NONE',  ( 0.000000000000000000, 0.000000000000000000, 0.000000000000000000 ) ) ;
#6720 = DIRECTION ( 'NONE',  ( 0.000000000000000000, -0.7071067811865535679, 0.7071067811865414665 ) ) ;
#6721 = VERTEX_POINT ( 'NONE', #15060 ) ;
#6722 = ORIENTED_EDGE ( 'NONE', *, *, #15173, .F. ) ;
#6723 = AXIS2_PLACEMENT_3D ( 'NONE', #10571, #1127, #11213 ) ;
#6724 = DIRECTION ( 'NONE',  ( 0.000000000000000000, 0.000000000000000000, -1.000000000000000000 ) ) ;
#6725 = CARTESIAN_POINT ( 'NONE',  ( 5.200000000000002842, 0.000000000000000000, -2.700000000000000622 ) ) ;
#6726 = DIRECTION ( 'NONE',  ( -1.000000000000000000, 0.000000000000000000, 0.000000000000000000 ) ) ;
#6727 = VERTEX_POINT ( 'NONE', #16491 ) ;
#6728 = ORIENTED_EDGE ( 'NONE', *, *, #9575, .F. ) ;
#6729 = CARTESIAN_POINT ( 'NONE',  ( 10.00000000000000000, 0.000000000000000000, 0.000000000000000000 ) ) ;
#6730 = VERTEX_POINT ( 'NONE', #15163 ) ;
#6731 = CARTESIAN_POINT ( 'NONE',  ( 10.00000000000000000, 1.017308535512385870, 56.37237871411034007 ) ) ;
#6732 = EDGE_CURVE ( 'NONE', #16786, #16509, #3729, .T. ) ;
#6733 = CARTESIAN_POINT ( 'NONE',  ( 4.000000000000000000, 2.309401076758515803, -0.4999999999999995559 ) ) ;
#6734 = CARTESIAN_POINT ( 'NONE',  ( 10.00000000000000000, -46.27827401617379621, -31.97297851452475470 ) ) ;
#6735 = VERTEX_POINT ( 'NONE', #971 ) ;
#6736 = CARTESIAN_POINT ( 'NONE',  ( -90.00000000009001155, -34.99999999999999289, 40.00000000000000000 ) ) ;
#6737 = AXIS2_PLACEMENT_3D ( 'NONE', #17449, #8504, #12100 ) ;
#6738 = EDGE_LOOP ( 'NONE', ( #8603, #8961, #10355, #7885 ) ) ;
#6739 = CARTESIAN_POINT ( 'NONE',  ( 1.287237434362044075, 3.875615274277557809, -3.430618716626812059 ) ) ;
#6740 = CARTESIAN_POINT ( 'NONE',  ( 10.00000000000000000, 0.000000000000000000, 0.000000000000000000 ) ) ;
#6741 = DIRECTION ( 'NONE',  ( -1.000000000000000000, -0.000000000000000000, -0.000000000000000000 ) ) ;
#6742 = EDGE_CURVE ( 'NONE', #1178, #6521, #2715, .T. ) ;
#6743 = ORIENTED_EDGE ( 'NONE', *, *, #17885, .T. ) ;
#6744 = FACE_OUTER_BOUND ( 'NONE', #18600, .T. ) ;
#6745 = ORIENTED_EDGE ( 'NONE', *, *, #3753, .F. ) ;
#6746 = DIRECTION ( 'NONE',  ( -1.000000000000000000, -0.000000000000000000, -0.000000000000000000 ) ) ;
#6747 = DIRECTION ( 'NONE',  ( 0.000000000000000000, -6.938893903900287191E-15, 1.000000000000000000 ) ) ;
#6748 = EDGE_LOOP ( 'NONE', ( #7631, #10378, #950, #8623, #15637 ) ) ;
#6749 = VERTEX_POINT ( 'NONE', #5045 ) ;
#6750 = CARTESIAN_POINT ( 'NONE',  ( -0.9999999999999986677, -27.60846790388774608, -2.000000000000000000 ) ) ;
#6751 = EDGE_CURVE ( 'NONE', #9771, #12049, #13365, .T. ) ;
#6752 = ORIENTED_EDGE ( 'NONE', *, *, #2185, .F. ) ;
#6753 = CARTESIAN_POINT ( 'NONE',  ( 0.000000000000000000, 0.000000000000000000, 0.000000000000000000 ) ) ;
#6754 = DIRECTION ( 'NONE',  ( 1.000000000000000000, 0.000000000000000000, 0.000000000000000000 ) ) ;
#6755 = AXIS2_PLACEMENT_3D ( 'NONE', #11426, #11336, #17154 ) ;
#6756 = EDGE_LOOP ( 'NONE', ( #4733, #11762, #2296, #16852 ) ) ;
#6757 = AXIS2_PLACEMENT_3D ( 'NONE', #14911, #1854, #17234 ) ;
#6758 = ORIENTED_EDGE ( 'NONE', *, *, #4003, .T. ) ;
#6759 = CYLINDRICAL_SURFACE ( 'NONE', #18149, 2.649999999999999467 ) ;
#6760 = CARTESIAN_POINT ( 'NONE',  ( 4.000000000000000000, -1.560351142792952617, -0.2242961665059816367 ) ) ;
#6761 = CARTESIAN_POINT ( 'NONE',  ( -10.00000000000000000, 0.000000000000000000, 0.000000000000000000 ) ) ;
#6762 = FACE_BOUND ( 'NONE', #12312, .T. ) ;
#6763 = AXIS2_PLACEMENT_3D ( 'NONE', #4654, #10456, #16272 ) ;
#6764 = CARTESIAN_POINT ( 'NONE',  ( 2.500000000000000000, -1.178949249685218081, -2.041999999999998039 ) ) ;
#6765 = DIRECTION ( 'NONE',  ( -1.000000000000000000, -0.000000000000000000, 0.000000000000000000 ) ) ;
#6766 = CARTESIAN_POINT ( 'NONE',  ( 4.144923636027600722, -29.35885059145708098, -2.000000000000000000 ) ) ;
#6767 = ORIENTED_EDGE ( 'NONE', *, *, #1346, .T. ) ;
#6768 = CARTESIAN_POINT ( 'NONE',  ( 0.000000000000000000, -40.58063702438316511, -39.14194549634407139 ) ) ;
#6769 = LINE ( 'NONE', #15088, #5662 ) ;
#6770 = DIRECTION ( 'NONE',  ( 0.000000000000000000, 0.000000000000000000, 1.000000000000000000 ) ) ;
#6771 = CARTESIAN_POINT ( 'NONE',  ( 5.200000000000002842, 3.061616997868383634E-16, -2.500000000000000444 ) ) ;
#6772 = CONTEXT_DEPENDENT_SHAPE_REPRESENTATION ( #9390, #1602 ) ;
#6773 = ORIENTED_EDGE ( 'NONE', *, *, #2374, .T. ) ;
#6774 = AXIS2_PLACEMENT_3D ( 'NONE', #6835, #18460, #8364 ) ;
#6775 = ORIENTED_EDGE ( 'NONE', *, *, #7358, .F. ) ;
#6776 = AXIS2_PLACEMENT_3D ( 'NONE', #137, #1646, #18452 ) ;
#6777 = AXIS2_PLACEMENT_3D ( 'NONE', #14577, #1532, #7334 ) ;
#6778 = EDGE_CURVE ( 'NONE', #10374, #5915, #3818, .T. ) ;
#6779 = EDGE_CURVE ( 'NONE', #3645, #2724, #15800, .T. ) ;
#6780 = VERTEX_POINT ( 'NONE', #2006 ) ;
#6781 = CYLINDRICAL_SURFACE ( 'NONE', #11150, 24.00000000002399858 ) ;
#6782 = EDGE_CURVE ( 'NONE', #8150, #15649, #18220, .T. ) ;
#6783 = CARTESIAN_POINT ( 'NONE',  ( 10.00000000000000000, 46.20417134726132247, 32.31183295104789011 ) ) ;
#6784 = CARTESIAN_POINT ( 'NONE',  ( 10.00000000000000000, 0.000000000000000000, 0.000000000000000000 ) ) ;
#6785 = FACE_OUTER_BOUND ( 'NONE', #734, .T. ) ;
#6786 = DIRECTION ( 'NONE',  ( 0.000000000000000000, -0.1564344650402170467, -0.9876883405951398798 ) ) ;
#6787 = EDGE_CURVE ( 'NONE', #11293, #1465, #12449, .T. ) ;
#6788 = CARTESIAN_POINT ( 'NONE',  ( 0.000000000000000000, 41.62350880771986539, -47.29147401531912465 ) ) ;
#6789 = DIRECTION ( 'NONE',  ( 1.000000000000000000, 0.000000000000000000, -0.000000000000000000 ) ) ;
#6790 = CARTESIAN_POINT ( 'NONE',  ( -4.249769933734879324, -30.10148593525447680, 0.000000000000000000 ) ) ;
#6791 = ORIENTED_EDGE ( 'NONE', *, *, #16460, .T. ) ;
#6792 = CYLINDRICAL_SURFACE ( 'NONE', #10296, 33.00000000003299760 ) ;
#6793 = VERTEX_POINT ( 'NONE', #6581 ) ;
#6794 = AXIS2_PLACEMENT_3D ( 'NONE', #2064, #13497, #7872 ) ;
#6795 = DIRECTION ( 'NONE',  ( 0.000000000000000000, 0.000000000000000000, -1.000000000000000000 ) ) ;
#6796 = FACE_OUTER_BOUND ( 'NONE', #14226, .T. ) ;
#6797 = ORIENTED_EDGE ( 'NONE', *, *, #1172, .T. ) ;
#6798 = EDGE_LOOP ( 'NONE', ( #4406, #10089, #8837, #6988 ) ) ;
#6799 = FACE_OUTER_BOUND ( 'NONE', #11488, .T. ) ;
#6800 = DIRECTION ( 'NONE',  ( 0.000000000000000000, 0.000000000000000000, 1.000000000000000000 ) ) ;
#6801 = ORIENTED_EDGE ( 'NONE', *, *, #4456, .F. ) ;
#6802 = ADVANCED_FACE ( 'NONE', ( #13638 ), #588, .T. ) ;
#6803 = EDGE_CURVE ( 'NONE', #17453, #4430, #17329, .T. ) ;
#6804 = FACE_OUTER_BOUND ( 'NONE', #7060, .T. ) ;
#6805 = ADVANCED_FACE ( 'NONE', ( #18006 ), #2285, .T. ) ;
#6806 = DIRECTION ( 'NONE',  ( 0.000000000000000000, 0.000000000000000000, -1.000000000000000000 ) ) ;
#6807 = CARTESIAN_POINT ( 'NONE',  ( -1.128893538851230005, 11.24999999999999467, 23.47286943213250154 ) ) ;
#6808 = DIRECTION ( 'NONE',  ( 0.000000000000000000, 1.000000000000000000, 0.000000000000000000 ) ) ;
#6809 = CARTESIAN_POINT ( 'NONE',  ( -90.00000000009001155, -49.14213562373095812, -1.301042606982603940E-15 ) ) ;
#6810 = ORIENTED_EDGE ( 'NONE', *, *, #754, .F. ) ;
#6811 = EDGE_CURVE ( 'NONE', #14782, #1295, #10922, .T. ) ;
#6812 = CARTESIAN_POINT ( 'NONE',  ( 1.144235203016666258, 3.958177651039090250, -0.09382832055445661235 ) ) ;
#6813 = CARTESIAN_POINT ( 'NONE',  ( 0.000000000000000000, 11.24999999999999467, 0.000000000000000000 ) ) ;
#6814 = DIRECTION ( 'NONE',  ( 0.000000000000000000, -0.9510565162951500895, -0.3090169943749581649 ) ) ;
#6815 = ORIENTED_EDGE ( 'NONE', *, *, #5855, .T. ) ;
#6816 = ORIENTED_EDGE ( 'NONE', *, *, #8524, .F. ) ;
#6817 = LINE ( 'NONE', #15583, #9912 ) ;
#6818 = SURFACE_STYLE_FILL_AREA ( #17117 ) ;
#6819 = ORIENTED_EDGE ( 'NONE', *, *, #1664, .F. ) ;
#6820 = CARTESIAN_POINT ( 'NONE',  ( -90.00000000009001155, 2.000000000000001776, -1.301042606982603940E-15 ) ) ;
#6821 = CARTESIAN_POINT ( 'NONE',  ( 10.00000000000000000, 1.335003989221626997, 56.23315539212691050 ) ) ;
#6822 = CARTESIAN_POINT ( 'NONE',  ( 13.90576474687263264, 10.00000000000000000, -42.79754323328189969 ) ) ;
#6823 = ORIENTED_EDGE ( 'NONE', *, *, #12399, .F. ) ;
#6824 = CARTESIAN_POINT ( 'NONE',  ( 0.3865131578947368918, -23.49682122285426189, 0.000000000000000000 ) ) ;
#6825 = VERTEX_POINT ( 'NONE', #886 ) ;
#6826 = CARTESIAN_POINT ( 'NONE',  ( 4.140404888673277384, 2.228338276487440428, -3.686887068327033390 ) ) ;
#6827 = FACE_OUTER_BOUND ( 'NONE', #7260, .T. ) ;
#6828 = DIRECTION ( 'NONE',  ( 0.000000000000000000, -0.3090169943749549453, 0.9510565162951511997 ) ) ;
#6829 = VECTOR ( 'NONE', #6545, 1000.000000000000000 ) ;
#6830 = ORIENTED_EDGE ( 'NONE', *, *, #12564, .F. ) ;
#6831 = FACE_OUTER_BOUND ( 'NONE', #10446, .T. ) ;
#6832 = ADVANCED_FACE ( 'NONE', ( #2196 ), #1649, .F. ) ;
#6833 = ORIENTED_EDGE ( 'NONE', *, *, #3120, .T. ) ;
#6834 = DIRECTION ( 'NONE',  ( 1.000000000000000000, 0.000000000000000000, -0.000000000000000000 ) ) ;
#6835 = CARTESIAN_POINT ( 'NONE',  ( 0.000000000000000000, -42.79754323328189969, -13.90576474687263264 ) ) ;
#6836 = ORIENTED_EDGE ( 'NONE', *, *, #6596, .T. ) ;
#6837 = ORIENTED_EDGE ( 'NONE', *, *, #18205, .T. ) ;
#6838 = DIRECTION ( 'NONE',  ( -1.000000000000000000, -0.000000000000000000, 0.000000000000000000 ) ) ;
#6839 = VERTEX_POINT ( 'NONE', #8662 ) ;
#6840 = LINE ( 'NONE', #17143, #2418 ) ;
#6841 = CARTESIAN_POINT ( 'NONE',  ( 10.04305231718579705, -34.99999999999999289, 30.90933677959249337 ) ) ;
#6842 = AXIS2_PLACEMENT_3D ( 'NONE', #523, #6329, #10700 ) ;
#6843 = CIRCLE ( 'NONE', #14451, 63.00000000006298961 ) ;
#6844 = AXIS2_PLACEMENT_3D ( 'NONE', #15133, #18169, #1975 ) ;
#6845 = EDGE_CURVE ( 'NONE', #1295, #7035, #599, .T. ) ;
#6846 = ORIENTED_EDGE ( 'NONE', *, *, #14720, .F. ) ;
#6847 = ADVANCED_FACE ( 'NONE', ( #1344 ), #12578, .F. ) ;
#6848 = ORIENTED_EDGE ( 'NONE', *, *, #4458, .F. ) ;
#6849 = DIRECTION ( 'NONE',  ( 0.000000000000000000, 0.000000000000000000, 1.000000000000000000 ) ) ;
#6850 = CARTESIAN_POINT ( 'NONE',  ( 0.000000000000000000, 40.70683587897958233, 38.81885513160002432 ) ) ;
#6851 = CARTESIAN_POINT ( 'NONE',  ( -117.1020693116506379, -30.00000000000000000, -19.69080595179801207 ) ) ;
#6852 = DIRECTION ( 'NONE',  ( 0.000000000000000000, 0.000000000000000000, 1.000000000000000000 ) ) ;
#6853 = VERTEX_POINT ( 'NONE', #5751 ) ;
#6854 = CARTESIAN_POINT ( 'NONE',  ( 0.000000000000000000, 16.45250512421934630, -53.92768374110874419 ) ) ;
#6855 = DIRECTION ( 'NONE',  ( 0.000000000000000000, -0.5877852522924802425, 0.8090169943749422332 ) ) ;
#6856 = CARTESIAN_POINT ( 'NONE',  ( 45.00000000000000000, 10.00000000000000000, -5.120903701083534543E-13 ) ) ;
#6857 = ORIENTED_EDGE ( 'NONE', *, *, #2302, .T. ) ;
#6858 = CARTESIAN_POINT ( 'NONE',  ( 10.04305231718579705, -30.00000000000000000, 28.25933677959249835 ) ) ;
#6859 = CIRCLE ( 'NONE', #13241, 2.649999999999992806 ) ;
#6860 = CARTESIAN_POINT ( 'NONE',  ( 10.00000000000000000, 0.000000000000000000, 0.000000000000000000 ) ) ;
#6861 = LINE ( 'NONE', #1348, #14867 ) ;
#6862 = CARTESIAN_POINT ( 'NONE',  ( 10.00000000000000000, 29.03656532225563680, 15.68049343256006800 ) ) ;
#6863 = ORIENTED_EDGE ( 'NONE', *, *, #6322, .T. ) ;
#6864 = CIRCLE ( 'NONE', #10813, 7.500000000000007105 ) ;
#6865 = AXIS2_PLACEMENT_3D ( 'NONE', #6221, #13188, #4522 ) ;
#6866 = ADVANCED_FACE ( 'NONE', ( #3927 ), #7135, .T. ) ;
#6867 = ORIENTED_EDGE ( 'NONE', *, *, #16913, .F. ) ;
#6868 = AXIS2_PLACEMENT_3D ( 'NONE', #17294, #10133, #8428 ) ;
#6869 = AXIS2_PLACEMENT_3D ( 'NONE', #1455, #6108, #16118 ) ;
#6870 = ORIENTED_EDGE ( 'NONE', *, *, #10960, .T. ) ;
#6871 = CARTESIAN_POINT ( 'NONE',  ( 0.000000000000000000, 0.000000000000000000, 0.000000000000000000 ) ) ;
#6872 = DIRECTION ( 'NONE',  ( -1.000000000000000000, 0.000000000000000000, -0.000000000000000000 ) ) ;
#6873 = DIRECTION ( 'NONE',  ( -1.000000000000000000, -0.000000000000000000, -0.000000000000000000 ) ) ;
#6874 = DIRECTION ( 'NONE',  ( -1.000000000000000000, 0.000000000000000000, -0.000000000000000000 ) ) ;
#6875 = DIRECTION ( 'NONE',  ( -1.000000000000000000, -0.000000000000000000, -0.000000000000000000 ) ) ;
#6876 = DIRECTION ( 'NONE',  ( 2.031314180040284764E-16, 1.000000000000000000, 1.301042606982601623E-16 ) ) ;
#6877 = CARTESIAN_POINT ( 'NONE',  ( 0.000000000000000000, 5.051668046482832750E-16, -4.000000000000000000 ) ) ;
#6878 = CIRCLE ( 'NONE', #18437, 24.00000000002399858 ) ;
#6879 = CARTESIAN_POINT ( 'NONE',  ( -36.40576474687271258, 0.000000000000000000, -26.45033635316118747 ) ) ;
#6880 = ORIENTED_EDGE ( 'NONE', *, *, #6989, .T. ) ;
#6881 = DIRECTION ( 'NONE',  ( -1.000000000000000000, 0.000000000000000000, 0.000000000000000000 ) ) ;
#6882 = AXIS2_PLACEMENT_3D ( 'NONE', #9727, #2484, #15629 ) ;
#6883 = ORIENTED_EDGE ( 'NONE', *, *, #3479, .F. ) ;
#6884 = AXIS2_PLACEMENT_3D ( 'NONE', #3558, #9538, #792 ) ;
#6885 = DIRECTION ( 'NONE',  ( 0.000000000000000000, -1.000000000000000000, 0.000000000000000000 ) ) ;
#6886 = CARTESIAN_POINT ( 'NONE',  ( 10.00000000000000000, -55.83748330407401284, -7.813799127873885197 ) ) ;
#6887 = VERTEX_POINT ( 'NONE', #18380 ) ;
#6888 = AXIS2_PLACEMENT_3D ( 'NONE', #7248, #4033, #1445 ) ;
#6889 = CIRCLE ( 'NONE', #1122, 2.500000000000000444 ) ;
#6890 = EDGE_CURVE ( 'NONE', #6965, #8582, #3642, .T. ) ;
#6891 = DIRECTION ( 'NONE',  ( -0.8660254037844377084, -0.5000000000000015543, 0.000000000000000000 ) ) ;
#6892 = CARTESIAN_POINT ( 'NONE',  ( -56.50000000009000445, -43.00000000000000000, 3.817814120399276590E-13 ) ) ;
#6894 = EDGE_CURVE ( 'NONE', #34, #12340, #17253, .T. ) ;
#6893 = DIRECTION ( 'NONE',  ( -1.000000000000000000, -0.000000000000000000, -0.000000000000000000 ) ) ;
#6895 = ORIENTED_EDGE ( 'NONE', *, *, #2704, .F. ) ;
#6896 = AXIS2_PLACEMENT_3D ( 'NONE', #8652, #14459, #14560 ) ;
#6897 =( GEOMETRIC_REPRESENTATION_CONTEXT ( 3 ) GLOBAL_UNCERTAINTY_ASSIGNED_CONTEXT ( ( #11083 ) ) GLOBAL_UNIT_ASSIGNED_CONTEXT ( ( #16851, #15422, #13994 ) ) REPRESENTATION_CONTEXT ( 'NONE', 'WORKASPACE' ) );
#6898 = DIRECTION ( 'NONE',  ( 0.000000000000000000, 0.000000000000000000, 1.000000000000000000 ) ) ;
#6899 = CARTESIAN_POINT ( 'NONE',  ( 4.198928548860774157, -0.8158838809860124996, -3.526471437616918170 ) ) ;
#6900 = CIRCLE ( 'NONE', #12685, 2.499999999999999556 ) ;
#6901 = AXIS2_PLACEMENT_3D ( 'NONE', #7078, #12709, #6800 ) ;
#6902 = CARTESIAN_POINT ( 'NONE',  ( 2.500000000000000000, 2.357898499370431722, -2.818925648462311528E-15 ) ) ;
#6903 = DIRECTION ( 'NONE',  ( 0.000000000000000000, 0.000000000000000000, 1.000000000000000000 ) ) ;
#6904 = ADVANCED_FACE ( 'NONE', ( #4017 ), #2733, .T. ) ;
#6905 = UNCERTAINTY_MEASURE_WITH_UNIT (LENGTH_MEASURE( 1.000000000000000082E-05 ), #2929, 'distance_accuracy_value', 'NONE');
#6906 = DIRECTION ( 'NONE',  ( -1.000000000000000000, 0.000000000000000000, -0.000000000000000000 ) ) ;
#6907 = VERTEX_POINT ( 'NONE', #18766 ) ;
#6908 = CARTESIAN_POINT ( 'NONE',  ( -117.1020693116506379, -38.00000000000000000, -22.34080595179800355 ) ) ;
#6909 = CARTESIAN_POINT ( 'NONE',  ( 0.000000000000000000, 61.47135697633778051, 13.79392154159156014 ) ) ;
#6910 = CARTESIAN_POINT ( 'NONE',  ( 0.000000000000000000, 0.000000000000000000, 0.000000000000000000 ) ) ;
#6911 = VERTEX_POINT ( 'NONE', #8298 ) ;
#6912 = ORIENTED_EDGE ( 'NONE', *, *, #16153, .F. ) ;
#6913 = EDGE_CURVE ( 'NONE', #24, #8001, #14302, .T. ) ;
#6914 = CARTESIAN_POINT ( 'NONE',  ( 0.000000000000000000, -10.11537145609416122, 55.33199130079781014 ) ) ;
#6915 = SURFACE_SIDE_STYLE ('',( #18629 ) ) ;
#6916 = AXIS2_PLACEMENT_3D ( 'NONE', #4651, #14379, #10453 ) ;
#6917 = EDGE_CURVE ( 'NONE', #10253, #16801, #12765, .T. ) ;
#6918 = VERTEX_POINT ( 'NONE', #6858 ) ;
#6919 = CYLINDRICAL_SURFACE ( 'NONE', #7294, 33.00000000003299760 ) ;
#6920 = AXIS2_PLACEMENT_3D ( 'NONE', #15572, #9557, #3964 ) ;
#6921 = CIRCLE ( 'NONE', #4779, 0.5155456020628804703 ) ;
#6922 = EDGE_CURVE ( 'NONE', #5103, #10364, #7293, .T. ) ;
#6923 = PRODUCT_DEFINITION_SHAPE ( 'NONE', 'NONE',  #12243 ) ;
#6924 = ADVANCED_FACE ( 'NONE', ( #8390 ), #17157, .T. ) ;
#6925 = CARTESIAN_POINT ( 'NONE',  ( 0.000000000000000000, -55.83748330407401284, 16.18620087215011338 ) ) ;
#6926 = CARTESIAN_POINT ( 'NONE',  ( 10.00000000000000000, 26.49895292618005271, 49.76630880786320432 ) ) ;
#6927 = ORIENTED_EDGE ( 'NONE', *, *, #5858, .F. ) ;
#6928 = LINE ( 'NONE', #11501, #12809 ) ;
#6929 = AXIS2_PLACEMENT_3D ( 'NONE', #420, #998, #15193 ) ;
#6930 = ADVANCED_FACE ( 'NONE', ( #5449 ), #4106, .T. ) ;
#6931 = AXIS2_PLACEMENT_3D ( 'NONE', #410, #17932, #4602 ) ;
#6932 = ORIENTED_EDGE ( 'NONE', *, *, #13644, .F. ) ;
#6934 = LINE ( 'NONE', #14164, #9647 ) ;
#6933 = PRODUCT_DEFINITION_CONTEXT ( 'detailed design', #2938, 'design' ) ;
#6935 = CARTESIAN_POINT ( 'NONE',  ( 10.00000000000000000, -5.876895005581972420, -62.72529079327814117 ) ) ;
#6936 = DIRECTION ( 'NONE',  ( 0.000000000000000000, -1.224646799147334718E-16, 1.000000000000000000 ) ) ;
#6937 = ORIENTED_EDGE ( 'NONE', *, *, #15298, .T. ) ;
#6938 = DIRECTION ( 'NONE',  ( 1.000000000000000000, -3.469446951953611231E-16, 0.000000000000000000 ) ) ;
#6939 = VERTEX_POINT ( 'NONE', #6967 ) ;
#6940 = DIRECTION ( 'NONE',  ( 0.000000000000000000, 0.000000000000000000, 1.000000000000000000 ) ) ;
#6941 = FACE_OUTER_BOUND ( 'NONE', #7812, .T. ) ;
#6942 = EDGE_LOOP ( 'NONE', ( #2639, #17115 ) ) ;
#6943 = ORIENTED_EDGE ( 'NONE', *, *, #11923, .T. ) ;
#6944 = CARTESIAN_POINT ( 'NONE',  ( 10.00000000000000000, 13.40641754777700534, -24.79895094899245933 ) ) ;
#6945 = ORIENTED_EDGE ( 'NONE', *, *, #17454, .F. ) ;
#6946 = CYLINDRICAL_SURFACE ( 'NONE', #10017, 12.00000000001200462 ) ;
#6947 = LINE ( 'NONE', #3714, #13447 ) ;
#6948 = CIRCLE ( 'NONE', #7245, 63.00000000006298961 ) ;
#6949 = CIRCLE ( 'NONE', #3300, 0.7499999999999997780 ) ;
#6950 = CONICAL_SURFACE ( 'NONE', #3923, 2.500000000000000888, 0.9599310885968785900 ) ;
#6951 = CIRCLE ( 'NONE', #8487, 2.700000000000000622 ) ;
#6952 = EDGE_CURVE ( 'NONE', #18105, #4975, #10324, .T. ) ;
#6953 = ORIENTED_EDGE ( 'NONE', *, *, #11097, .T. ) ;
#6954 = AXIS2_PLACEMENT_3D ( 'NONE', #6219, #3278, #17567 ) ;
#6955 = ORIENTED_EDGE ( 'NONE', *, *, #6641, .F. ) ;
#6956 = CYLINDRICAL_SURFACE ( 'NONE', #3854, 24.00000000002400213 ) ;
#6957 = CARTESIAN_POINT ( 'NONE',  ( -4.211140560182196957, -2.431303136016552013, -3.745885042887436178 ) ) ;
#6958 = FACE_BOUND ( 'NONE', #7211, .T. ) ;
#6959 = DIRECTION ( 'NONE',  ( -1.000000000000000000, 0.000000000000000000, 0.000000000000000000 ) ) ;
#6960 = CONICAL_SURFACE ( 'NONE', #4838, 4.000000000000000000, 0.8911886515913786111 ) ;
#6961 = DIRECTION ( 'NONE',  ( 1.000000000000000000, 0.000000000000000000, 0.000000000000000000 ) ) ;
#6962 = DIRECTION ( 'NONE',  ( 0.000000000000000000, 0.000000000000000000, 1.000000000000000000 ) ) ;
#6963 = VECTOR ( 'NONE', #6479, 1000.000000000000000 ) ;
#6964 = LINE ( 'NONE', #4015, #17779 ) ;
#6965 = VERTEX_POINT ( 'NONE', #8488 ) ;
#6966 = AXIS2_PLACEMENT_3D ( 'NONE', #8363, #1038, #7980 ) ;
#6967 = CARTESIAN_POINT ( 'NONE',  ( 10.00000000000000000, -44.70888270294135936, -34.13306034420235591 ) ) ;
#6968 = B_SPLINE_CURVE_WITH_KNOTS ( 'NONE', 3,
 ( #1902, #12640, #5300, #11108, #9688 ),
 .UNSPECIFIED., .F., .F.,
 ( 4, 1, 4 ),
 ( 0.000000000000000000, 0.002309401076758505356, 0.004618802153517010713 ),
 .UNSPECIFIED. ) ;
#6969 = LINE ( 'NONE', #972, #4146 ) ;
#6970 = CARTESIAN_POINT ( 'NONE',  ( 10.00000000000000000, 0.000000000000000000, 0.000000000000000000 ) ) ;
#6971 = ORIENTED_EDGE ( 'NONE', *, *, #1334, .F. ) ;
#6972 = ORIENTED_EDGE ( 'NONE', *, *, #15774, .T. ) ;
#6973 = AXIS2_PLACEMENT_3D ( 'NONE', #16578, #13729, #16867 ) ;
#6974 = EDGE_CURVE ( 'NONE', #14902, #18755, #3041, .T. ) ;
#6975 = AXIS2_PLACEMENT_3D ( 'NONE', #7592, #14931, #1874 ) ;
#6976 = ORIENTED_EDGE ( 'NONE', *, *, #7706, .F. ) ;
#6977 = DIRECTION ( 'NONE',  ( -1.000000000000000000, 0.000000000000000000, -0.000000000000000000 ) ) ;
#6978 = DIRECTION ( 'NONE',  ( 0.000000000000000000, 1.000000000000000000, 0.000000000000000000 ) ) ;
#6979 = ORIENTED_EDGE ( 'NONE', *, *, #14464, .F. ) ;
#6980 = DIRECTION ( 'NONE',  ( -1.000000000000000000, 0.000000000000000000, 0.000000000000000000 ) ) ;
#6981 = CYLINDRICAL_SURFACE ( 'NONE', #7493, 24.00000000002399858 ) ;
#6982 = CYLINDRICAL_SURFACE ( 'NONE', #3272, 56.24900000005625600 ) ;
#6983 = CIRCLE ( 'NONE', #17626, 12.00000000001200462 ) ;
#6984 = DIRECTION ( 'NONE',  ( 1.000000000000000000, 0.000000000000000000, 0.000000000000000000 ) ) ;
#6985 = DIRECTION ( 'NONE',  ( 0.000000000000000000, 0.000000000000000000, -1.000000000000000000 ) ) ;
#6986 = ORIENTED_EDGE ( 'NONE', *, *, #13834, .F. ) ;
#6987 = CARTESIAN_POINT ( 'NONE',  ( 0.000000000000000000, 0.000000000000000000, 0.000000000000000000 ) ) ;
#6988 = ORIENTED_EDGE ( 'NONE', *, *, #17068, .F. ) ;
#6989 = EDGE_CURVE ( 'NONE', #12311, #8822, #294, .T. ) ;
#6990 = AXIS2_PLACEMENT_3D ( 'NONE', #18345, #7013, #8536 ) ;
#6991 = DIRECTION ( 'NONE',  ( 0.000000000000000000, 0.000000000000000000, 1.000000000000000000 ) ) ;
#6992 = VERTEX_POINT ( 'NONE', #14573 ) ;
#6993 = CARTESIAN_POINT ( 'NONE',  ( 0.000000000000000000, 24.68609584167159454, 50.69000562871650573 ) ) ;
#6994 = CARTESIAN_POINT ( 'NONE',  ( -79.64793068852898728, -43.00000000000000000, -31.86039329588756530 ) ) ;
#6995 = ADVANCED_FACE ( 'NONE', ( #11892 ), #10561, .F. ) ;
#6996 = CARTESIAN_POINT ( 'NONE',  ( 10.00000000000000000, -40.70683587897985234, 38.81885513159974010 ) ) ;
#6997 = ORIENTED_EDGE ( 'NONE', *, *, #12752, .F. ) ;
#6998 = VECTOR ( 'NONE', #18033, 1000.000000000000000 ) ;
#6999 = AXIS2_PLACEMENT_3D ( 'NONE', #322, #5843, #11930 ) ;
#7000 = FACE_BOUND ( 'NONE', #11546, .T. ) ;
#7001 = PLANE ( 'NONE',  #933 ) ;
#7002 = CARTESIAN_POINT ( 'NONE',  ( 0.000000000000000000, 0.000000000000000000, 0.000000000000000000 ) ) ;
#7003 = CARTESIAN_POINT ( 'NONE',  ( 10.00000000000000000, -14.19907017806883864, 22.07705612348834734 ) ) ;
#7004 = LINE ( 'NONE', #2719, #18496 ) ;
#7005 = ORIENTED_EDGE ( 'NONE', *, *, #1104, .T. ) ;
#7006 = DIRECTION ( 'NONE',  ( 0.000000000000000000, 0.000000000000000000, 1.000000000000000000 ) ) ;
#7007 = DIRECTION ( 'NONE',  ( 0.9995004958639132076, 0.000000000000000000, 0.03160314490350067673 ) ) ;
#7008 = DIRECTION ( 'NONE',  ( 0.000000000000000000, -0.9510565162951565288, 0.3090169943749384029 ) ) ;
#7009 = EDGE_LOOP ( 'NONE', ( #1266, #2906, #8230, #1013 ) ) ;
#7010 = VERTEX_POINT ( 'NONE', #17434 ) ;
#7011 = CARTESIAN_POINT ( 'NONE',  ( 0.000000000000000000, 20.32630374611185786, 16.60877409751175904 ) ) ;
#7012 = ORIENTED_EDGE ( 'NONE', *, *, #11152, .T. ) ;
#7013 = DIRECTION ( 'NONE',  ( -0.000000000000000000, -0.000000000000000000, -1.000000000000000000 ) ) ;
#7014 = CARTESIAN_POINT ( 'NONE',  ( 2.500000000000000000, -1.768423874527823569, 1.021000000000002350 ) ) ;
#7015 = DIRECTION ( 'NONE',  ( 0.000000000000000000, -0.9510565162951502005, -0.3090169943749579984 ) ) ;
#7016 = EDGE_CURVE ( 'NONE', #1879, #14399, #2427, .T. ) ;
#7017 = ORIENTED_EDGE ( 'NONE', *, *, #6680, .T. ) ;
#7018 = EDGE_CURVE ( 'NONE', #10477, #14440, #16415, .T. ) ;
#7020 = AXIS2_PLACEMENT_3D ( 'NONE', #8584, #14398, #11550 ) ;
#7019 = FACE_OUTER_BOUND ( 'NONE', #12880, .T. ) ;
#7021 = EDGE_CURVE ( 'NONE', #13113, #560, #1806, .T. ) ;
#7022 = VERTEX_POINT ( 'NONE', #15999 ) ;
#7023 = DIRECTION ( 'NONE',  ( 0.000000000000000000, 0.000000000000000000, -1.000000000000000000 ) ) ;
#7024 = CARTESIAN_POINT ( 'NONE',  ( -4.888507282057958037, -29.45674523562211888, -2.000000000000000000 ) ) ;
#7025 = DIRECTION ( 'NONE',  ( 1.000000000000000000, 0.000000000000000000, 0.000000000000000000 ) ) ;
#7026 = ORIENTED_EDGE ( 'NONE', *, *, #9236, .F. ) ;
#7027 = DIRECTION ( 'NONE',  ( 1.000000000000000000, 0.000000000000000000, -0.000000000000000000 ) ) ;
#7028 = ORIENTED_EDGE ( 'NONE', *, *, #7697, .T. ) ;
#7029 = ADVANCED_FACE ( 'NONE', ( #13339 ), #11714, .T. ) ;
#7030 = CARTESIAN_POINT ( 'NONE',  ( 2.500000000000000000, 2.357898499370431722, -2.818925648462311528E-15 ) ) ;
#7031 = DIRECTION ( 'NONE',  ( -0.000000000000000000, 1.000000000000000000, -0.000000000000000000 ) ) ;
#7032 = ORIENTED_EDGE ( 'NONE', *, *, #11424, .F. ) ;
#7033 = VERTEX_POINT ( 'NONE', #106 ) ;
#7034 = DIRECTION ( 'NONE',  ( -1.000000000000000000, 0.000000000000000000, 0.000000000000000000 ) ) ;
#7035 = VERTEX_POINT ( 'NONE', #4565 ) ;
#7036 = DIRECTION ( 'NONE',  ( -1.000000000000000000, 0.000000000000000000, 0.000000000000000000 ) ) ;
#7037 = CARTESIAN_POINT ( 'NONE',  ( -90.40196296004810961, 1.745901168134654787E-14, 6.951864913735149365 ) ) ;
#7038 = VECTOR ( 'NONE', #10622, 1000.000000000000000 ) ;
#7039 = ADVANCED_FACE ( 'NONE', ( #7613 ), #10459, .T. ) ;
#7040 = VERTEX_POINT ( 'NONE', #2959 ) ;
#7041 = EDGE_CURVE ( 'NONE', #4390, #5560, #6382, .T. ) ;
#7042 = ORIENTED_EDGE ( 'NONE', *, *, #10843, .F. ) ;
#7043 = LINE ( 'NONE', #4198, #17854 ) ;
#7044 = CARTESIAN_POINT ( 'NONE',  ( -2.449848172108560540, -3.432307619358754724, -3.503702292528910078 ) ) ;
#7045 = CARTESIAN_POINT ( 'NONE',  ( 10.00000000000000000, 22.76987570971561325, -23.88582760061456511 ) ) ;
#7046 = DIRECTION ( 'NONE',  ( 0.000000000000000000, 0.000000000000000000, 1.000000000000000000 ) ) ;
#7047 = CIRCLE ( 'NONE', #17651, 2.649999999999999467 ) ;
#7048 = CYLINDRICAL_SURFACE ( 'NONE', #16396, 12.00000000001200817 ) ;
#7049 = CYLINDRICAL_SURFACE ( 'NONE', #5549, 23.50000000000000355 ) ;
#7050 = DIRECTION ( 'NONE',  ( -0.000000000000000000, 1.000000000000000000, -0.000000000000000000 ) ) ;
#7051 = EDGE_LOOP ( 'NONE', ( #1370, #7896, #653, #17908 ) ) ;
#7052 = CARTESIAN_POINT ( 'NONE',  ( -11.15000000000000391, 0.000000000000000000, 0.000000000000000000 ) ) ;
#7053 = EDGE_CURVE ( 'NONE', #13562, #6419, #6983, .T. ) ;
#7054 = DIRECTION ( 'NONE',  ( 0.000000000000000000, 0.000000000000000000, 1.000000000000000000 ) ) ;
#7055 = TOROIDAL_SURFACE ( 'NONE', #4019, 2.700000000000000622, 0.2000000000000000111 ) ;
#7056 = AXIS2_PLACEMENT_3D ( 'NONE', #15325, #15613, #14288 ) ;
#7057 = DIRECTION ( 'NONE',  ( -2.031314180040284764E-16, -1.000000000000000000, -1.301042606982601377E-16 ) ) ;
#7058 = DIRECTION ( 'NONE',  ( -1.000000000000000000, 0.000000000000000000, 0.000000000000000000 ) ) ;
#7059 = ORIENTED_EDGE ( 'NONE', *, *, #14529, .F. ) ;
#7060 = EDGE_LOOP ( 'NONE', ( #526, #768, #17611, #1701 ) ) ;
#7062 = FACE_OUTER_BOUND ( 'NONE', #14190, .T. ) ;
#7061 = CIRCLE ( 'NONE', #6755, 2.649999999999999467 ) ;
#7063 = DIRECTION ( 'NONE',  ( -0.9873298794253686506, 1.799126239882929340E-16, 0.1586811557617576196 ) ) ;
#7064 = VERTEX_POINT ( 'NONE', #10375 ) ;
#7065 = CARTESIAN_POINT ( 'NONE',  ( 10.00000000000000000, -24.46385708179976604, -9.514709542737152859 ) ) ;
#7066 = CYLINDRICAL_SURFACE ( 'NONE', #5361, 24.00000000002400213 ) ;
#7067 = LINE ( 'NONE', #12891, #245 ) ;
#7068 = DIRECTION ( 'NONE',  ( 1.000000000000000000, 0.000000000000000000, 0.000000000000000000 ) ) ;
#7069 = LINE ( 'NONE', #17277, #16282 ) ;
#7070 = EDGE_LOOP ( 'NONE', ( #13061, #13508, #14373, #13028 ) ) ;
#7071 = DIRECTION ( 'NONE',  ( 0.000000000000000000, 0.000000000000000000, -1.000000000000000000 ) ) ;
#7072 = ORIENTED_EDGE ( 'NONE', *, *, #3039, .T. ) ;
#7073 = ADVANCED_FACE ( 'NONE', ( #9135 ), #5813, .F. ) ;
#7074 = CARTESIAN_POINT ( 'NONE',  ( -36.40576474687247099, 10.00000000000000000, 26.45033635316149301 ) ) ;
#7075 = ORIENTED_EDGE ( 'NONE', *, *, #13500, .F. ) ;
#7076 = SHAPE_DEFINITION_REPRESENTATION ( #9060, #18682 ) ;
#7077 = VECTOR ( 'NONE', #15695, 1000.000000000000000 ) ;
#7078 = CARTESIAN_POINT ( 'NONE',  ( 10.04305231718579705, -30.00000000000000000, 30.90933677959249337 ) ) ;
#7079 = ORIENTED_EDGE ( 'NONE', *, *, #2726, .F. ) ;
#7080 = AXIS2_PLACEMENT_3D ( 'NONE', #1932, #16229, #13745 ) ;
#7081 =( REPRESENTATION_RELATIONSHIP ('NONE','NONE', #11014, #1770 ) REPRESENTATION_RELATIONSHIP_WITH_TRANSFORMATION ( #8691 )SHAPE_REPRESENTATION_RELATIONSHIP( ) );
#7082 = ADVANCED_FACE ( 'NONE', ( #11625 ), #8754, .F. ) ;
#7083 = CARTESIAN_POINT ( 'NONE',  ( 0.000000000000000000, 22.07705612348839708, 14.19907017806876048 ) ) ;
#7084 = CARTESIAN_POINT ( 'NONE',  ( 4.197393957002303999, -0.4069871074557456780, -3.503767560748925813 ) ) ;
#7085 = DIRECTION ( 'NONE',  ( 0.000000000000000000, 0.000000000000000000, 1.000000000000000000 ) ) ;
#7086 = CARTESIAN_POINT ( 'NONE',  ( 0.000000000000000000, 1.305124410222461284, 0.000000000000000000 ) ) ;
#7087 = EDGE_CURVE ( 'NONE', #8855, #18145, #8811, .T. ) ;
#7088 = AXIS2_PLACEMENT_3D ( 'NONE', #15632, #3931, #4109 ) ;
#7089 = DIRECTION ( 'NONE',  ( -1.000000000000000000, -0.000000000000000000, 0.000000000000000000 ) ) ;
#7090 = ORIENTED_EDGE ( 'NONE', *, *, #3166, .T. ) ;
#7091 = DIRECTION ( 'NONE',  ( -1.000000000000000000, -0.000000000000000000, 0.000000000000000000 ) ) ;
#7092 = CARTESIAN_POINT ( 'NONE',  ( 1.567478505476134606E-15, 4.618802153517012066, -5.000000000000000000 ) ) ;
#7093 = CARTESIAN_POINT ( 'NONE',  ( -10.00000000000000000, 0.000000000000000000, 0.000000000000000000 ) ) ;
#7094 = ORIENTED_EDGE ( 'NONE', *, *, #16704, .F. ) ;
#7095 = ORIENTED_EDGE ( 'NONE', *, *, #11569, .T. ) ;
#7096 = DIRECTION ( 'NONE',  ( 1.000000000000000000, -2.312964634635740492E-16, 0.000000000000000000 ) ) ;
#7097 = ORIENTED_EDGE ( 'NONE', *, *, #1661, .T. ) ;
#7098 = AXIS2_PLACEMENT_3D ( 'NONE', #3184, #9174, #14800 ) ;
#7099 = CARTESIAN_POINT ( 'NONE',  ( 0.000000000000000000, 7.813799127873274131, 55.83748330407410521 ) ) ;
#7100 = DIRECTION ( 'NONE',  ( -0.000000000000000000, 1.000000000000000000, -0.000000000000000000 ) ) ;
#7101 = EDGE_LOOP ( 'NONE', ( #4700, #16166, #10209, #3872 ) ) ;
#7102 = CARTESIAN_POINT ( 'NONE',  ( -79.64793068852927149, -34.99999999999999289, 34.51039329588763849 ) ) ;
#7103 = VERTEX_POINT ( 'NONE', #3054 ) ;
#7104 = UNCERTAINTY_MEASURE_WITH_UNIT (LENGTH_MEASURE( 1.000000000000000082E-05 ), #11384, 'distance_accuracy_value', 'NONE');
#7105 = LINE ( 'NONE', #14436, #16049 ) ;
#7106 = ORIENTED_EDGE ( 'NONE', *, *, #16473, .T. ) ;
#7107 = CARTESIAN_POINT ( 'NONE',  ( 0.000000000000000000, 3.000000000000000000, -55.00000000000000000 ) ) ;
#7108 = ORIENTED_EDGE ( 'NONE', *, *, #9592, .T. ) ;
#7109 = CARTESIAN_POINT ( 'NONE',  ( 10.00000000000000000, 16.45250512421856470, 53.92768374110897156 ) ) ;
#7110 = DIRECTION ( 'NONE',  ( -1.000000000000000000, 0.000000000000000000, -0.000000000000000000 ) ) ;
#7111 = EDGE_LOOP ( 'NONE', ( #1597, #8219 ) ) ;
#7112 = ORIENTED_EDGE ( 'NONE', *, *, #15654, .F. ) ;
#7113 = CARTESIAN_POINT ( 'NONE',  ( -79.64793068852898728, -34.99999999999999289, -29.21039329588757383 ) ) ;
#7114 = SURFACE_STYLE_FILL_AREA ( #9437 ) ;
#7115 = ORIENTED_EDGE ( 'NONE', *, *, #10843, .T. ) ;
#7116 = DIRECTION ( 'NONE',  ( -0.000000000000000000, -0.000000000000000000, 1.000000000000000000 ) ) ;
#7117 = LINE ( 'NONE', #11948, #366 ) ;
#7118 = EDGE_CURVE ( 'NONE', #5630, #10460, #7417, .T. ) ;
#7119 = EDGE_CURVE ( 'NONE', #9531, #13493, #193, .T. ) ;
#7120 = COLOUR_RGB ( '',1.000000000000000000, 0.9490196078431372140, 0.9098039215686274384 ) ;
#7121 = PRODUCT_DEFINITION ( 'UNKNOWN', '', #14751, #5410 ) ;
#7122 = CARTESIAN_POINT ( 'NONE',  ( 5.021051876504148963E-15, -26.50000000000000000, 41.00000000000000000 ) ) ;
#7123 = VERTEX_POINT ( 'NONE', #17619 ) ;
#7124 = EDGE_CURVE ( 'NONE', #5282, #7169, #16723, .T. ) ;
#7125 = VERTEX_POINT ( 'NONE', #17899 ) ;
#7126 = CARTESIAN_POINT ( 'NONE',  ( -2.000000000000006661, 3.464101615137750834, 0.000000000000000000 ) ) ;
#7127 = CARTESIAN_POINT ( 'NONE',  ( 2.500000000000000444, 0.000000000000000000, -25.03750572909317285 ) ) ;
#7128 = CARTESIAN_POINT ( 'NONE',  ( 0.000000000000000000, 0.000000000000000000, -4.484454397937119197 ) ) ;
#7129 = DIRECTION ( 'NONE',  ( 0.000000000000000000, -1.000000000000000000, 0.000000000000000000 ) ) ;
#7130 = EDGE_CURVE ( 'NONE', #18246, #3993, #18237, .T. ) ;
#7131 = CARTESIAN_POINT ( 'NONE',  ( 4.799999999999999822, 0.000000000000000000, -1.000000000000000000 ) ) ;
#7132 = DIRECTION ( 'NONE',  ( 0.000000000000000000, 0.000000000000000000, 1.000000000000000000 ) ) ;
#7133 = CARTESIAN_POINT ( 'NONE',  ( 4.154306624730763176, -2.398490048084970461, -3.721999068284303824 ) ) ;
#7134 = ORIENTED_EDGE ( 'NONE', *, *, #4575, .T. ) ;
#7135 = CYLINDRICAL_SURFACE ( 'NONE', #11252, 5.000000000000004441 ) ;
#7136 = DIRECTION ( 'NONE',  ( -1.000000000000000000, 0.000000000000000000, 0.000000000000000000 ) ) ;
#7137 = AXIS2_PLACEMENT_3D ( 'NONE', #2046, #10511, #17756 ) ;
#7138 = ORIENTED_EDGE ( 'NONE', *, *, #1557, .T. ) ;
#7139 = CARTESIAN_POINT ( 'NONE',  ( 10.00000000000000000, 7.478235706488965739, 55.74967257055886449 ) ) ;
#7140 = DIRECTION ( 'NONE',  ( 0.000000000000000000, 0.000000000000000000, 1.000000000000000000 ) ) ;
#7141 = AXIS2_PLACEMENT_3D ( 'NONE', #6376, #7691, #12183 ) ;
#7142 = AXIS2_PLACEMENT_3D ( 'NONE', #17785, #1693, #13140 ) ;
#7143 = EDGE_CURVE ( 'NONE', #607, #5984, #10026, .T. ) ;
#7144 = CONTEXT_DEPENDENT_SHAPE_REPRESENTATION ( #15851, #92 ) ;
#7145 = EDGE_CURVE ( 'NONE', #6377, #3492, #12456, .T. ) ;
#7146 = ORIENTED_EDGE ( 'NONE', *, *, #11461, .T. ) ;
#7147 = EDGE_CURVE ( 'NONE', #15934, #743, #5779, .T. ) ;
#7148 = EDGE_CURVE ( 'NONE', #15064, #91, #17337, .T. ) ;
#7149 = VERTEX_POINT ( 'NONE', #6633 ) ;
#7150 = LINE ( 'NONE', #5782, #3271 ) ;
#7151 = CARTESIAN_POINT ( 'NONE',  ( -90.72413394419160682, -10.00000000000001954, 4.947285117213268357 ) ) ;
#7152 = FACE_OUTER_BOUND ( 'NONE', #13311, .T. ) ;
#7153 = ORIENTED_EDGE ( 'NONE', *, *, #9395, .F. ) ;
#7154 = CIRCLE ( 'NONE', #5334, 24.00000000002399858 ) ;
#7155 = CARTESIAN_POINT ( 'NONE',  ( 0.000000000000000000, -50.69000562871624993, -24.68609584167212745 ) ) ;
#7156 = DIRECTION ( 'NONE',  ( -1.000000000000000000, -0.000000000000000000, -0.000000000000000000 ) ) ;
#7157 = FACE_OUTER_BOUND ( 'NONE', #11019, .T. ) ;
#7158 = CYLINDRICAL_SURFACE ( 'NONE', #3827, 12.00000000001200462 ) ;
#7159 = ORIENTED_EDGE ( 'NONE', *, *, #11389, .F. ) ;
#7160 = LINE ( 'NONE', #12987, #9400 ) ;
#7161 = VERTEX_POINT ( 'NONE', #9861 ) ;
#7162 = CYLINDRICAL_SURFACE ( 'NONE', #9658, 63.00000000006298961 ) ;
#7163 = EDGE_LOOP ( 'NONE', ( #15544, #17477, #5599, #16458 ) ) ;
#7164 = CIRCLE ( 'NONE', #8690, 24.00000000002399858 ) ;
#7165 = ITEM_DEFINED_TRANSFORMATION ( 'NONE', 'NONE', #8949,  #8017 ) ;
#7166 = EDGE_LOOP ( 'NONE', ( #6728, #8929 ) ) ;
#7167 = CIRCLE ( 'NONE', #2915, 30.00000000000000000 ) ;
#7168 = ADVANCED_FACE ( 'NONE', ( #18429 ), #18340, .T. ) ;
#7169 = VERTEX_POINT ( 'NONE', #5288 ) ;
#7170 = DIRECTION ( 'NONE',  ( 0.000000000000000000, 0.000000000000000000, 1.000000000000000000 ) ) ;
#7171 = CARTESIAN_POINT ( 'NONE',  ( 10.00000000000000000, -55.83748330407413363, 7.813799127873079620 ) ) ;
#7172 = AXIS2_PLACEMENT_3D ( 'NONE', #15021, #15118, #2070 ) ;
#7173 = VECTOR ( 'NONE', #10780, 1000.000000000000000 ) ;
#7174 = CARTESIAN_POINT ( 'NONE',  ( 12.49999999999999289, 0.000000000000000000, 0.000000000000000000 ) ) ;
#7175 = DIRECTION ( 'NONE',  ( -1.000000000000000000, -0.000000000000000000, -0.000000000000000000 ) ) ;
#7176 = VECTOR ( 'NONE', #18784, 1000.000000000000000 ) ;
#7177 = VECTOR ( 'NONE', #8336, 1000.000000000000000 ) ;
#7178 = VECTOR ( 'NONE', #13966, 1000.000000000000000 ) ;
#7179 = LINE ( 'NONE', #2897, #15152 ) ;
#7180 = CIRCLE ( 'NONE', #4153, 0.7499999999999997780 ) ;
#7181 = ORIENTED_EDGE ( 'NONE', *, *, #9130, .F. ) ;
#7182 = CARTESIAN_POINT ( 'NONE',  ( -31.74999999999995737, 3.061616997868383634E-16, -2.500000000000000444 ) ) ;
#7183 = FACE_OUTER_BOUND ( 'NONE', #9734, .T. ) ;
#7184 = DIRECTION ( 'NONE',  ( 0.000000000000000000, 0.000000000000000000, 1.000000000000000000 ) ) ;
#7185 = ORIENTED_EDGE ( 'NONE', *, *, #9430, .F. ) ;
#7186 = VERTEX_POINT ( 'NONE', #8253 ) ;
#7187 = APPLICATION_CONTEXT ( 'automotive_design' ) ;
#7188 = CYLINDRICAL_SURFACE ( 'NONE', #14775, 2.396904916527699214 ) ;
#7189 = SHAPE_REPRESENTATION_RELATIONSHIP ( 'NONE' , 'NONE' ,  #16765, #13523 ) ;
#7190 = EDGE_LOOP ( 'NONE', ( #2256, #12555, #5937, #13819 ) ) ;
#7191 = CIRCLE ( 'NONE', #16923, 33.00000000003299760 ) ;
#7192 = AXIS2_PLACEMENT_3D ( 'NONE', #1043, #2179, #18565 ) ;
#7193 = CIRCLE ( 'NONE', #837, 33.00000000003299760 ) ;
#7194 = AXIS2_PLACEMENT_3D ( 'NONE', #6210, #12012, #17829 ) ;
#7195 = AXIS2_PLACEMENT_3D ( 'NONE', #1052, #18759, #15620 ) ;
#7196 = EDGE_CURVE ( 'NONE', #18189, #7033, #11089, .T. ) ;
#7197 = LINE ( 'NONE', #5684, #15682 ) ;
#7198 = CARTESIAN_POINT ( 'NONE',  ( 13.90576474687263264, 10.00000000000000000, -40.14754323328190111 ) ) ;
#7199 = ORIENTED_EDGE ( 'NONE', *, *, #5486, .T. ) ;
#7200 = AXIS2_PLACEMENT_3D ( 'NONE', #12769, #5612, #18575 ) ;
#7201 = ORIENTED_EDGE ( 'NONE', *, *, #12482, .T. ) ;
#7202 = DIRECTION ( 'NONE',  ( 0.000000000000000000, -0.000000000000000000, -1.000000000000000000 ) ) ;
#7203 = ORIENTED_EDGE ( 'NONE', *, *, #7723, .T. ) ;
#7204 = CARTESIAN_POINT ( 'NONE',  ( 1.567478505476134606E-15, 4.618802153517012066, -3.433295621305382905 ) ) ;
#7205 = ORIENTED_EDGE ( 'NONE', *, *, #17403, .T. ) ;
#7206 = CIRCLE ( 'NONE', #2966, 5.000000000000004441 ) ;
#7207 = LINE ( 'NONE', #8551, #2711 ) ;
#7208 = DIRECTION ( 'NONE',  ( 0.000000000000000000, 0.000000000000000000, -1.000000000000000000 ) ) ;
#7209 = AXIS2_PLACEMENT_3D ( 'NONE', #13202, #155, #10345 ) ;
#7210 = VERTEX_POINT ( 'NONE', #10998 ) ;
#7211 = EDGE_LOOP ( 'NONE', ( #5632, #16300 ) ) ;
#7212 = CIRCLE ( 'NONE', #2345, 24.00000000002400213 ) ;
#7213 = EDGE_CURVE ( 'NONE', #8606, #3467, #5389, .T. ) ;
#7214 = DIRECTION ( 'NONE',  ( 0.000000000000000000, 0.8910065241883654563, 0.4539904997395512454 ) ) ;
#7215 = SHAPE_REPRESENTATION_RELATIONSHIP ( 'NONE' , 'NONE' ,  #5670, #8303 ) ;
#7216 = EDGE_LOOP ( 'NONE', ( #3968, #9071, #15983, #1117 ) ) ;
#7217 = DIRECTION ( 'NONE',  ( 1.000000000000000000, 0.000000000000000000, 0.000000000000000000 ) ) ;
#7218 = EDGE_CURVE ( 'NONE', #9150, #2599, #12442, .T. ) ;
#7219 = AXIS2_PLACEMENT_3D ( 'NONE', #4291, #8928, #4558 ) ;
#7220 = AXIS2_PLACEMENT_3D ( 'NONE', #9365, #5264, #6708 ) ;
#7221 = FACE_OUTER_BOUND ( 'NONE', #4555, .T. ) ;
#7222 = ORIENTED_EDGE ( 'NONE', *, *, #16221, .F. ) ;
#7223 = PRODUCT_DEFINITION_SHAPE ( 'NONE', 'NONE',  #18844 ) ;
#7224 = ORIENTED_EDGE ( 'NONE', *, *, #7457, .T. ) ;
#7225 = CARTESIAN_POINT ( 'NONE',  ( -10.00000000000000000, 0.000000000000000000, 0.000000000000000000 ) ) ;
#7226 = DIRECTION ( 'NONE',  ( 0.000000000000000000, 0.000000000000000000, 1.000000000000000000 ) ) ;
#7227 = DIRECTION ( 'NONE',  ( 0.000000000000000000, 0.000000000000000000, 1.000000000000000000 ) ) ;
#7228 = CARTESIAN_POINT ( 'NONE',  ( 2.500000000000000000, 2.357898499370431722, -2.818925648462311528E-15 ) ) ;
#7229 = CYLINDRICAL_SURFACE ( 'NONE', #12694, 2.649999999999992806 ) ;
#7230 = EDGE_CURVE ( 'NONE', #16509, #2331, #13091, .T. ) ;
#7231 = CARTESIAN_POINT ( 'NONE',  ( 0.000000000000000000, 0.000000000000000000, 0.000000000000000000 ) ) ;
#7232 = CARTESIAN_POINT ( 'NONE',  ( -56.50000000009000445, -30.00000000000000000, 3.817814120399276590E-13 ) ) ;
#7233 = CIRCLE ( 'NONE', #18482, 0.7500000000000000000 ) ;
#7234 = CARTESIAN_POINT ( 'NONE',  ( -1.312671235360383548, -3.860931062424228788, -0.05923475698271369466 ) ) ;
#7235 = ORIENTED_EDGE ( 'NONE', *, *, #8831, .T. ) ;
#7236 = DIRECTION ( 'NONE',  ( -1.000000000000000000, 0.000000000000000000, -0.000000000000000000 ) ) ;
#7237 = DIRECTION ( 'NONE',  ( -0.000000000000000000, -1.000000000000000000, -0.000000000000000000 ) ) ;
#7238 = CIRCLE ( 'NONE', #3603, 2.500000000000000444 ) ;
#7239 = VERTEX_POINT ( 'NONE', #11194 ) ;
#7240 = CARTESIAN_POINT ( 'NONE',  ( -90.00000000009001155, -34.99999999999999289, -10.00000000000001066 ) ) ;
#7241 = FACE_OUTER_BOUND ( 'NONE', #17969, .T. ) ;
#7242 = AXIS2_PLACEMENT_3D ( 'NONE', #17105, #16813, #4055 ) ;
#7243 = AXIS2_PLACEMENT_3D ( 'NONE', #481, #12671, #10948 ) ;
#7244 = ORIENTED_EDGE ( 'NONE', *, *, #754, .T. ) ;
#7245 = AXIS2_PLACEMENT_3D ( 'NONE', #12050, #8911, #10350 ) ;
#7246 = ORIENTED_EDGE ( 'NONE', *, *, #17825, .F. ) ;
#7247 = AXIS2_PLACEMENT_3D ( 'NONE', #17622, #10289, #14576 ) ;
#7248 = CARTESIAN_POINT ( 'NONE',  ( -10.00000000000000000, 0.000000000000000000, 0.000000000000000000 ) ) ;
#7249 = LINE ( 'NONE', #8773, #13119 ) ;
#7250 = PRESENTATION_LAYER_ASSIGNMENT (  '', '', ( #13042 ) ) ;
#7251 = ORIENTED_EDGE ( 'NONE', *, *, #11860, .F. ) ;
#7252 = AXIS2_PLACEMENT_3D ( 'NONE', #563, #16183, #17702 ) ;
#7253 = DIRECTION ( 'NONE',  ( 0.000000000000000000, -0.3090169943749349613, -0.9510565162951576390 ) ) ;
#7254 = EDGE_CURVE ( 'NONE', #684, #38, #16735, .T. ) ;
#7255 = CARTESIAN_POINT ( 'NONE',  ( 10.00000000000000000, 0.000000000000000000, 0.000000000000000000 ) ) ;
#7256 = EDGE_CURVE ( 'NONE', #16127, #17356, #14913, .T. ) ;
#7257 = EDGE_CURVE ( 'NONE', #11551, #1152, #10940, .T. ) ;
#7258 = DIRECTION ( 'NONE',  ( -0.000000000000000000, 1.000000000000000000, -0.000000000000000000 ) ) ;
#7259 = LINE ( 'NONE', #8683, #5657 ) ;
#7260 = EDGE_LOOP ( 'NONE', ( #13047, #7873, #6060, #12947 ) ) ;
#7261 = CARTESIAN_POINT ( 'NONE',  ( 10.04305231718579705, -26.50000000000000000, 28.25933677959249835 ) ) ;
#7262 = ORIENTED_EDGE ( 'NONE', *, *, #12990, .F. ) ;
#7263 = EDGE_CURVE ( 'NONE', #8465, #15167, #2242, .T. ) ;
#7264 = FACE_OUTER_BOUND ( 'NONE', #4128, .T. ) ;
#7265 = DIRECTION ( 'NONE',  ( 0.000000000000000000, 0.000000000000000000, -1.000000000000000000 ) ) ;
#7266 = CIRCLE ( 'NONE', #16390, 24.00000000002399503 ) ;
#7267 = ORIENTED_EDGE ( 'NONE', *, *, #272, .T. ) ;
#7268 = APPLICATION_PROTOCOL_DEFINITION ( 'draft international standard', 'automotive_design', 1998, #14371 ) ;
#7269 = AXIS2_PLACEMENT_3D ( 'NONE', #9601, #13898, #7987 ) ;
#7270 = EDGE_CURVE ( 'NONE', #6793, #4158, #13968, .T. ) ;
#7271 = ORIENTED_EDGE ( 'NONE', *, *, #8537, .T. ) ;
#7272 = EDGE_CURVE ( 'NONE', #16587, #18040, #307, .T. ) ;
#7273 = AXIS2_PLACEMENT_3D ( 'NONE', #7030, #5877, #13031 ) ;
#7274 = EDGE_CURVE ( 'NONE', #10666, #18659, #21, .T. ) ;
#7275 = VERTEX_POINT ( 'NONE', #831 ) ;
#7276 = CARTESIAN_POINT ( 'NONE',  ( 50.00005079999999680, 6.799999999999999822, -1.500000000000000000 ) ) ;
#7277 = DIRECTION ( 'NONE',  ( 1.000000000000000000, 0.000000000000000000, 0.000000000000000000 ) ) ;
#7278 = CIRCLE ( 'NONE', #1794, 26.24900000002624978 ) ;
#7279 = DIRECTION ( 'NONE',  ( -1.000000000000000000, 0.000000000000000000, 0.000000000000000000 ) ) ;
#7280 = CARTESIAN_POINT ( 'NONE',  ( 11.25000000000000000, 0.000000000000000000, 0.000000000000000000 ) ) ;
#7281 = EDGE_CURVE ( 'NONE', #6583, #4502, #13393, .T. ) ;
#7282 = VECTOR ( 'NONE', #2095, 1000.000000000000114 ) ;
#7283 = DIRECTION ( 'NONE',  ( -0.000000000000000000, 1.000000000000000000, -0.000000000000000000 ) ) ;
#7284 = ORIENTED_EDGE ( 'NONE', *, *, #4813, .T. ) ;
#7285 = DIRECTION ( 'NONE',  ( -1.000000000000000000, 0.000000000000000000, -0.000000000000000000 ) ) ;
#7286 = DIRECTION ( 'NONE',  ( 0.000000000000000000, 0.000000000000000000, 1.000000000000000000 ) ) ;
#7287 = CYLINDRICAL_SURFACE ( 'NONE', #7300, 33.00000000003299760 ) ;
#7288 = ORIENTED_EDGE ( 'NONE', *, *, #13615, .T. ) ;
#7289 = EDGE_LOOP ( 'NONE', ( #6171, #4281 ) ) ;
#7290 = ADVANCED_FACE ( 'NONE', ( #14618 ), #3009, .F. ) ;
#7291 = FACE_BOUND ( 'NONE', #15923, .T. ) ;
#7292 = ORIENTED_EDGE ( 'NONE', *, *, #744, .T. ) ;
#7293 = CIRCLE ( 'NONE', #1216, 24.00000000002400569 ) ;
#7294 = AXIS2_PLACEMENT_3D ( 'NONE', #937, #11203, #9965 ) ;
#7295 = LINE ( 'NONE', #17581, #16906 ) ;
#7296 = CARTESIAN_POINT ( 'NONE',  ( 0.000000000000000000, 24.79895094899259789, 13.40641754777674421 ) ) ;
#7297 = CARTESIAN_POINT ( 'NONE',  ( 0.000000000000000000, 12.18267823974751352, 25.42247726998019530 ) ) ;
#7298 = ORIENTED_EDGE ( 'NONE', *, *, #18560, .F. ) ;
#7299 = FACE_OUTER_BOUND ( 'NONE', #9687, .T. ) ;
#7300 = AXIS2_PLACEMENT_3D ( 'NONE', #11380, #13107, #17387 ) ;
#7301 = ORIENTED_EDGE ( 'NONE', *, *, #5854, .T. ) ;
#7302 = B_SPLINE_CURVE_WITH_KNOTS ( 'NONE', 3,
 ( #13514, #2088, #7893, #14945, #7786, #3139, #10371, #13426 ),
 .UNSPECIFIED., .F., .F.,
 ( 4, 2, 2, 4 ),
 ( 2.465131517071610173E-07, 0.001183067374689837636, 0.001774477805458902699, 0.002365888236227967761 ),
 .UNSPECIFIED. ) ;
#7303 = PRODUCT_DEFINITION_CONTEXT ( 'detailed design', #11199, 'design' ) ;
#7304 = CARTESIAN_POINT ( 'NONE',  ( 0.2500000000000002220, 0.000000000000000000, 0.000000000000000000 ) ) ;
#7305 = ORIENTED_EDGE ( 'NONE', *, *, #5386, .F. ) ;
#7306 = ORIENTED_EDGE ( 'NONE', *, *, #3841, .T. ) ;
#7307 = CIRCLE ( 'NONE', #14914, 33.00000000003299760 ) ;
#7308 = DIRECTION ( 'NONE',  ( -0.000000000000000000, 1.000000000000000000, -0.000000000000000000 ) ) ;
#7309 = DIRECTION ( 'NONE',  ( 2.031314180040284764E-16, 1.000000000000000000, 1.301042606982601377E-16 ) ) ;
#7310 = ORIENTED_EDGE ( 'NONE', *, *, #6438, .F. ) ;
#7311 = ORIENTED_EDGE ( 'NONE', *, *, #235, .F. ) ;
#7312 = ADVANCED_FACE ( 'NONE', ( #5673 ), #1572, .T. ) ;
#7313 = CARTESIAN_POINT ( 'NONE',  ( 0.000000000000000000, -27.94286728106395756, 3.730438010304225394 ) ) ;
#7314 = VERTEX_POINT ( 'NONE', #5936 ) ;
#7315 = CARTESIAN_POINT ( 'NONE',  ( 13.90576474687299680, 0.000000000000000000, 45.44754323328179169 ) ) ;
#7316 = AXIS2_PLACEMENT_3D ( 'NONE', #2022, #6406, #8014 ) ;
#7317 = CARTESIAN_POINT ( 'NONE',  ( 13.90576474687299680, 10.00000000000000000, 45.44754323328179169 ) ) ;
#7318 = EDGE_LOOP ( 'NONE', ( #11275, #8171, #18426, #16369 ) ) ;
#7319 = VERTEX_POINT ( 'NONE', #8708 ) ;
#7320 = DIRECTION ( 'NONE',  ( -1.000000000000000000, -0.000000000000000000, -0.000000000000000000 ) ) ;
#7321 = FACE_BOUND ( 'NONE', #6109, .T. ) ;
#7322 = DIRECTION ( 'NONE',  ( 1.000000000000000000, 0.000000000000000000, 0.000000000000000000 ) ) ;
#7323 = ORIENTED_EDGE ( 'NONE', *, *, #2362, .F. ) ;
#7324 = DIRECTION ( 'NONE',  ( -1.000000000000000000, 0.000000000000000000, 0.000000000000000000 ) ) ;
#7325 = EDGE_CURVE ( 'NONE', #13928, #16309, #8222, .T. ) ;
#7326 = DIRECTION ( 'NONE',  ( -1.000000000000000000, 0.000000000000000000, -0.000000000000000000 ) ) ;
#7327 = FACE_OUTER_BOUND ( 'NONE', #7598, .T. ) ;
#7328 = LINE ( 'NONE', #15908, #6574 ) ;
#7329 = ORIENTED_EDGE ( 'NONE', *, *, #7962, .T. ) ;
#7330 = CARTESIAN_POINT ( 'NONE',  ( 0.000000000000000000, 0.000000000000000000, 0.000000000000000000 ) ) ;
#7331 = CYLINDRICAL_SURFACE ( 'NONE', #16023, 12.00000000001200462 ) ;
#7332 = ORIENTED_EDGE ( 'NONE', *, *, #11664, .T. ) ;
#7333 = DIRECTION ( 'NONE',  ( -0.000000000000000000, 1.000000000000000000, -0.000000000000000000 ) ) ;
#7334 = DIRECTION ( 'NONE',  ( 0.000000000000000000, 0.000000000000000000, -1.000000000000000000 ) ) ;
#7335 = ORIENTED_EDGE ( 'NONE', *, *, #18370, .F. ) ;
#7336 = AXIS2_PLACEMENT_3D ( 'NONE', #7086, #17381, #1201 ) ;
#7337 = DIRECTION ( 'NONE',  ( 0.000000000000000000, 0.000000000000000000, 1.000000000000000000 ) ) ;
#7338 = CYLINDRICAL_SURFACE ( 'NONE', #7020, 56.24900000005625600 ) ;
#7339 = VERTEX_POINT ( 'NONE', #5851 ) ;
#7340 = CARTESIAN_POINT ( 'NONE',  ( 0.000000000000000000, 2.357898499370431722, -2.818925648462311528E-15 ) ) ;
#7341 = FACE_BOUND ( 'NONE', #6942, .T. ) ;
#7342 = VECTOR ( 'NONE', #10473, 1000.000000000000000 ) ;
#7343 = DIRECTION ( 'NONE',  ( -1.000000000000000000, 0.000000000000000000, 0.000000000000000000 ) ) ;
#7344 = CARTESIAN_POINT ( 'NONE',  ( -3.309651814758565180, -5.455921364805393026, -1.000000000000000000 ) ) ;
#7345 = DIRECTION ( 'NONE',  ( -1.000000000000000000, 0.000000000000000000, 0.000000000000000000 ) ) ;
#7346 = EDGE_LOOP ( 'NONE', ( #11154, #18223, #3566, #16661 ) ) ;
#7347 = DIRECTION ( 'NONE',  ( -1.000000000000000000, -0.000000000000000000, 0.000000000000000000 ) ) ;
#7348 = ORIENTED_EDGE ( 'NONE', *, *, #3913, .T. ) ;
#7349 = CARTESIAN_POINT ( 'NONE',  ( 0.000000000000000000, -40.58063702438372644, 39.14194549634347453 ) ) ;
#7350 = CYLINDRICAL_SURFACE ( 'NONE', #16676, 24.00000000002399858 ) ;
#7351 = VERTEX_POINT ( 'NONE', #2903 ) ;
#7352 = PRODUCT_CONTEXT ( 'NONE', #1115, 'mechanical' ) ;
#7353 = VERTEX_POINT ( 'NONE', #17306 ) ;
#7354 = EDGE_CURVE ( 'NONE', #3048, #8307, #5785, .T. ) ;
#7355 = CIRCLE ( 'NONE', #11322, 25.10000000000000142 ) ;
#7356 = EDGE_CURVE ( 'NONE', #7635, #18122, #10143, .T. ) ;
#7357 = CARTESIAN_POINT ( 'NONE',  ( 10.00000000000000000, 0.000000000000000000, 0.000000000000000000 ) ) ;
#7358 = EDGE_CURVE ( 'NONE', #14848, #806, #7597, .T. ) ;
#7359 = CARTESIAN_POINT ( 'NONE',  ( 4.024499207728848837, 2.323545700935681246, -3.572172305156870564 ) ) ;
#7360 = CARTESIAN_POINT ( 'NONE',  ( -10.00000000000000000, 0.000000000000000000, 0.000000000000000000 ) ) ;
#7361 = DIRECTION ( 'NONE',  ( 0.000000000000000000, 0.000000000000000000, 1.000000000000000000 ) ) ;
#7362 = EDGE_CURVE ( 'NONE', #6404, #4385, #14518, .T. ) ;
#7363 = DIRECTION ( 'NONE',  ( -1.000000000000000000, -0.000000000000000000, 0.000000000000000000 ) ) ;
#7364 = CYLINDRICAL_SURFACE ( 'NONE', #10132, 63.00000000006298961 ) ;
#7365 = CARTESIAN_POINT ( 'NONE',  ( 0.000000000000000000, -53.89344778774800204, -16.10733642026540124 ) ) ;
#7366 = VERTEX_POINT ( 'NONE', #14339 ) ;
#7367 = FILL_AREA_STYLE ('',( #6130 ) ) ;
#7368 = ADVANCED_FACE ( 'NONE', ( #2813 ), #12822, .T. ) ;
#7369 = DIRECTION ( 'NONE',  ( -1.000000000000000000, 0.000000000000000000, 0.000000000000000000 ) ) ;
#7370 = CIRCLE ( 'NONE', #4349, 24.00000000002399858 ) ;
#7371 = DIRECTION ( 'NONE',  ( -1.000000000000000000, -0.000000000000000000, -0.000000000000000000 ) ) ;
#7372 = ORIENTED_EDGE ( 'NONE', *, *, #141, .T. ) ;
#7373 = EDGE_LOOP ( 'NONE', ( #2556, #15033, #10077, #1817 ) ) ;
#7374 = CARTESIAN_POINT ( 'NONE',  ( 0.000000000000000000, -56.37237871411032586, -1.017308535512989609 ) ) ;
#7375 = ORIENTED_EDGE ( 'NONE', *, *, #11344, .T. ) ;
#7376 = ADVANCED_FACE ( 'NONE', ( #2623 ), #7287, .T. ) ;
#7377 = EDGE_CURVE ( 'NONE', #9315, #16736, #18551, .T. ) ;
#7378 = PRODUCT_DEFINITION_SHAPE ( 'NONE', 'NONE',  #18837 ) ;
#7379 = ADVANCED_FACE ( 'NONE', ( #2723 ), #17472, .T. ) ;
#7380 = VECTOR ( 'NONE', #7309, 1000.000000000000000 ) ;
#7381 = CARTESIAN_POINT ( 'NONE',  ( -10.00000000000000000, 0.000000000000000000, 0.000000000000000000 ) ) ;
#7382 = EDGE_CURVE ( 'NONE', #17073, #17166, #12780, .T. ) ;
#7383 = LINE ( 'NONE', #14628, #6538 ) ;
#7384 = AXIS2_PLACEMENT_3D ( 'NONE', #11162, #15263, #16994 ) ;
#7385 = AXIS2_PLACEMENT_3D ( 'NONE', #5242, #1167, #4022 ) ;
#7386 = DIRECTION ( 'NONE',  ( 0.000000000000000000, 0.000000000000000000, 1.000000000000000000 ) ) ;
#7387 = EDGE_CURVE ( 'NONE', #9886, #6276, #10041, .T. ) ;
#7388 = ORIENTED_EDGE ( 'NONE', *, *, #14622, .F. ) ;
#7389 = CARTESIAN_POINT ( 'NONE',  ( 3.061616997868383043E-15, -13.75000000000000533, -25.00000000000000000 ) ) ;
#7390 = CIRCLE ( 'NONE', #14973, 24.00000000002399503 ) ;
#7391 = ORIENTED_EDGE ( 'NONE', *, *, #16562, .T. ) ;
#7392 = CARTESIAN_POINT ( 'NONE',  ( 10.00000000000000000, -26.20671763660629594, 1.489278925039428936 ) ) ;
#7393 = ORIENTED_EDGE ( 'NONE', *, *, #4143, .T. ) ;
#7394 = VERTEX_POINT ( 'NONE', #18624 ) ;
#7395 = CARTESIAN_POINT ( 'NONE',  ( 10.00000000000000000, -1.489278925039700052, 26.20671763660628173 ) ) ;
#7396 = CARTESIAN_POINT ( 'NONE',  ( 0.2500000000000002220, 0.000000000000000000, 0.000000000000000000 ) ) ;
#7397 = EDGE_LOOP ( 'NONE', ( #2560, #5178, #11606, #17546 ) ) ;
#7398 = ORIENTED_EDGE ( 'NONE', *, *, #1151, .F. ) ;
#7399 = CARTESIAN_POINT ( 'NONE',  ( -36.40576474687271258, 0.000000000000000000, -23.80033635316118890 ) ) ;
#7400 = SURFACE_STYLE_FILL_AREA ( #16258 ) ;
#7401 = AXIS2_PLACEMENT_3D ( 'NONE', #910, #6885, #18512 ) ;
#7402 = ORIENTED_EDGE ( 'NONE', *, *, #8304, .T. ) ;
#7403 = FACE_OUTER_BOUND ( 'NONE', #17770, .T. ) ;
#7404 = FACE_OUTER_BOUND ( 'NONE', #12295, .T. ) ;
#7405 = EDGE_CURVE ( 'NONE', #12797, #13152, #9738, .T. ) ;
#7406 = VERTEX_POINT ( 'NONE', #5774 ) ;
#7407 = ORIENTED_EDGE ( 'NONE', *, *, #986, .F. ) ;
#7408 = DIRECTION ( 'NONE',  ( -0.01515971714484241721, 0.000000000000000000, 0.9998850848853023665 ) ) ;
#7409 = DIRECTION ( 'NONE',  ( 0.000000000000000000, 0.000000000000000000, -1.000000000000000000 ) ) ;
#7410 = DIRECTION ( 'NONE',  ( 1.000000000000000000, 0.000000000000000000, 0.000000000000000000 ) ) ;
#7411 = EDGE_LOOP ( 'NONE', ( #2751, #9487, #16289, #17680 ) ) ;
#7412 = CARTESIAN_POINT ( 'NONE',  ( 12.49999999999999289, 0.000000000000000000, -28.00000000000000711 ) ) ;
#7413 = CARTESIAN_POINT ( 'NONE',  ( 50.00005079999999680, 3.673940397442059178E-15, -30.00000000000000000 ) ) ;
#7414 = DIRECTION ( 'NONE',  ( -1.000000000000000000, 0.000000000000000000, 0.000000000000000000 ) ) ;
#7415 = PLANE ( 'NONE',  #13584 ) ;
#7416 = ORIENTED_EDGE ( 'NONE', *, *, #15357, .T. ) ;
#7417 = LINE ( 'NONE', #13234, #2 ) ;
#7418 = FILL_AREA_STYLE ('',( #17525 ) ) ;
#7419 = ORIENTED_EDGE ( 'NONE', *, *, #4070, .T. ) ;
#7420 = CARTESIAN_POINT ( 'NONE',  ( 0.000000000000000000, 48.50907078259382388, 40.19788616105627455 ) ) ;
#7421 = DIRECTION ( 'NONE',  ( -1.000000000000000000, 0.000000000000000000, -0.000000000000000000 ) ) ;
#7422 = EDGE_CURVE ( 'NONE', #15264, #1945, #11584, .T. ) ;
#7423 = EDGE_CURVE ( 'NONE', #16256, #3146, #17638, .T. ) ;
#7424 = ORIENTED_EDGE ( 'NONE', *, *, #12368, .F. ) ;
#7425 = DIRECTION ( 'NONE',  ( -0.000000000000000000, -0.000000000000000000, 1.000000000000000000 ) ) ;
#7426 = FACE_OUTER_BOUND ( 'NONE', #14178, .T. ) ;
#7427 = VERTEX_POINT ( 'NONE', #1751 ) ;
#7428 = CARTESIAN_POINT ( 'NONE',  ( 10.00000000000000000, 0.000000000000000000, 0.000000000000000000 ) ) ;
#7429 = CARTESIAN_POINT ( 'NONE',  ( 10.00000000000000000, -40.70683587897985234, 38.81885513159974010 ) ) ;
#7430 =( GEOMETRIC_REPRESENTATION_CONTEXT ( 3 ) GLOBAL_UNCERTAINTY_ASSIGNED_CONTEXT ( ( #254 ) ) GLOBAL_UNIT_ASSIGNED_CONTEXT ( ( #934, #2627, #11002 ) ) REPRESENTATION_CONTEXT ( 'NONE', 'WORKASPACE' ) );
#7431 = CARTESIAN_POINT ( 'NONE',  ( 10.00000000000000000, -55.74967257055877212, -7.478235706489567924 ) ) ;
#7432 = CARTESIAN_POINT ( 'NONE',  ( 10.00000000000000000, 24.68609584167159454, 50.69000562871650573 ) ) ;
#7433 = DIRECTION ( 'NONE',  ( 0.000000000000000000, 0.000000000000000000, 1.000000000000000000 ) ) ;
#7434 = VERTEX_POINT ( 'NONE', #4896 ) ;
#7435 = CARTESIAN_POINT ( 'NONE',  ( 0.000000000000000000, 47.29147401531955097, 41.62350880771938222 ) ) ;
#7436 = ORIENTED_EDGE ( 'NONE', *, *, #16999, .F. ) ;
#7437 = AXIS2_PLACEMENT_3D ( 'NONE', #6740, #2357, #8071 ) ;
#7438 =( NAMED_UNIT ( * ) PLANE_ANGLE_UNIT ( ) SI_UNIT ( $, .RADIAN. ) );
#7439 = CARTESIAN_POINT ( 'NONE',  ( 10.00000000000000000, -20.32630374611196800, 16.60877409751161693 ) ) ;
#7440 = ORIENTED_EDGE ( 'NONE', *, *, #4305, .F. ) ;
#7441 = ADVANCED_FACE ( 'NONE', ( #1652 ), #7461, .F. ) ;
#7442 = SHAPE_DEFINITION_REPRESENTATION ( #6923, #2517 ) ;
#7443 = ORIENTED_EDGE ( 'NONE', *, *, #10297, .T. ) ;
#7444 = ADVANCED_FACE ( 'NONE', ( #4612 ), #7565, .T. ) ;
#7445 = AXIS2_PLACEMENT_3D ( 'NONE', #17006, #16720, #12603 ) ;
#7446 = AXIS2_PLACEMENT_3D ( 'NONE', #8992, #12042, #3108 ) ;
#7447 = CIRCLE ( 'NONE', #15675, 24.00000000002399858 ) ;
#7448 = CARTESIAN_POINT ( 'NONE',  ( 10.00000000000000000, 0.000000000000000000, 0.000000000000000000 ) ) ;
#7449 = DIRECTION ( 'NONE',  ( 1.000000000000000000, 0.000000000000000000, 0.000000000000000000 ) ) ;
#7450 = DIRECTION ( 'NONE',  ( 0.1305261922200516844, -0.9914448613738103822, 0.000000000000000000 ) ) ;
#7451 = CYLINDRICAL_SURFACE ( 'NONE', #9434, 2.649999999999992806 ) ;
#7452 = CARTESIAN_POINT ( 'NONE',  ( 1.734723475976807094E-15, 4.618802153517012954, -0.4999999999999995559 ) ) ;
#7453 = DIRECTION ( 'NONE',  ( 1.000000000000000000, 0.000000000000000000, 0.000000000000000000 ) ) ;
#7454 = AXIS2_PLACEMENT_3D ( 'NONE', #642, #9112, #10717 ) ;
#7455 = CARTESIAN_POINT ( 'NONE',  ( 10.00000000000000000, 0.000000000000000000, 0.000000000000000000 ) ) ;
#7456 = ORIENTED_EDGE ( 'NONE', *, *, #1219, .F. ) ;
#7457 = EDGE_CURVE ( 'NONE', #14680, #2243, #1165, .T. ) ;
#7458 = EDGE_CURVE ( 'NONE', #1332, #7103, #5407, .T. ) ;
#7459 = DIRECTION ( 'NONE',  ( 0.000000000000000000, -0.3090169943749349613, -0.9510565162951576390 ) ) ;
#7460 = DIRECTION ( 'NONE',  ( 0.000000000000000000, 0.000000000000000000, -1.000000000000000000 ) ) ;
#7461 = CYLINDRICAL_SURFACE ( 'NONE', #6307, 2.649999999999995914 ) ;
#7462 = VERTEX_POINT ( 'NONE', #10609 ) ;
#7463 = AXIS2_PLACEMENT_3D ( 'NONE', #7099, #1579, #68 ) ;
#7464 = VERTEX_POINT ( 'NONE', #2041 ) ;
#7465 = CIRCLE ( 'NONE', #1998, 63.00000000006298961 ) ;
#7466 = DIRECTION ( 'NONE',  ( 0.000000000000000000, 1.000000000000000000, 0.000000000000000000 ) ) ;
#7467 =( NAMED_UNIT ( * ) SI_UNIT ( $, .STERADIAN. ) SOLID_ANGLE_UNIT ( ) );
#7468 = DIRECTION ( 'NONE',  ( 0.000000000000000000, 0.000000000000000000, -1.000000000000000000 ) ) ;
#7469 = EDGE_LOOP ( 'NONE', ( #6722, #9798, #385, #4740 ) ) ;
#7470 = CIRCLE ( 'NONE', #18736, 2.649999999999992806 ) ;
#7471 = AXIS2_PLACEMENT_3D ( 'NONE', #5450, #6416, #17076 ) ;
#7472 = CARTESIAN_POINT ( 'NONE',  ( 0.000000000000000000, 0.000000000000000000, 0.000000000000000000 ) ) ;
#7473 = CARTESIAN_POINT ( 'NONE',  ( 0.000000000000000000, 0.000000000000000000, 0.000000000000000000 ) ) ;
#7474 = EDGE_CURVE ( 'NONE', #8506, #7504, #15148, .T. ) ;
#7475 = AXIS2_PLACEMENT_3D ( 'NONE', #9252, #16310, #7551 ) ;
#7477 = AXIS2_PLACEMENT_3D ( 'NONE', #14747, #1700, #7514 ) ;
#7476 = DIRECTION ( 'NONE',  ( -1.000000000000000000, 0.000000000000000000, 0.000000000000000000 ) ) ;
#7478 = ORIENTED_EDGE ( 'NONE', *, *, #8039, .T. ) ;
#7479 = DIRECTION ( 'NONE',  ( 0.000000000000000000, 0.000000000000000000, 1.000000000000000000 ) ) ;
#7480 = ORIENTED_EDGE ( 'NONE', *, *, #8880, .F. ) ;
#7481 = PRODUCT_DEFINITION_CONTEXT ( 'detailed design', #8877, 'design' ) ;
#7482 = CARTESIAN_POINT ( 'NONE',  ( -79.64793068852927149, -30.00000000000000000, 31.86039329588764701 ) ) ;
#7483 = ORIENTED_EDGE ( 'NONE', *, *, #17625, .F. ) ;
#7484 = EDGE_CURVE ( 'NONE', #3414, #9474, #2353, .T. ) ;
#7485 = EDGE_CURVE ( 'NONE', #13348, #16644, #16054, .T. ) ;
#7486 = EDGE_CURVE ( 'NONE', #14160, #17232, #16145, .T. ) ;
#7487 = CYLINDRICAL_SURFACE ( 'NONE', #11133, 24.00000000002399858 ) ;
#7488 = CARTESIAN_POINT ( 'NONE',  ( 0.000000000000000000, -30.00000000000000000, 0.000000000000000000 ) ) ;
#7489 = CIRCLE ( 'NONE', #14477, 40.00000000000000000 ) ;
#7490 = ORIENTED_EDGE ( 'NONE', *, *, #14415, .T. ) ;
#7491 = ORIENTED_EDGE ( 'NONE', *, *, #15401, .F. ) ;
#7492 = DIRECTION ( 'NONE',  ( -1.000000000000000000, -0.000000000000000000, 0.000000000000000000 ) ) ;
#7493 = AXIS2_PLACEMENT_3D ( 'NONE', #14401, #12981, #14111 ) ;
#7494 = EDGE_CURVE ( 'NONE', #13122, #7406, #9347, .T. ) ;
#7495 = ORIENTED_EDGE ( 'NONE', *, *, #5277, .T. ) ;
#7496 = DIRECTION ( 'NONE',  ( -0.000000000000000000, 1.000000000000000000, 0.000000000000000000 ) ) ;
#7497 = CIRCLE ( 'NONE', #2633, 2.649999999999999467 ) ;
#7498 = EDGE_CURVE ( 'NONE', #18077, #6730, #6132, .T. ) ;
#7499 = EDGE_CURVE ( 'NONE', #16517, #7974, #14706, .T. ) ;
#7500 = CARTESIAN_POINT ( 'NONE',  ( 10.00000000000000000, -9.823366686500245137, -55.51919907100663920 ) ) ;
#7501 = VECTOR ( 'NONE', #3808, 1000.000000000000000 ) ;
#7502 = ORIENTED_EDGE ( 'NONE', *, *, #11323, .F. ) ;
#7503 = AXIS2_PLACEMENT_3D ( 'NONE', #3784, #11008, #16744 ) ;
#7504 = VERTEX_POINT ( 'NONE', #3098 ) ;
#7505 = DIRECTION ( 'NONE',  ( 0.000000000000000000, -1.000000000000000000, 0.000000000000000000 ) ) ;
#7506 = CIRCLE ( 'NONE', #13294, 56.24900000005625600 ) ;
#7507 = DIRECTION ( 'NONE',  ( 1.000000000000000000, 0.000000000000000000, 0.000000000000000000 ) ) ;
#7508 = CYLINDRICAL_SURFACE ( 'NONE', #16033, 26.24900000002624978 ) ;
#7509 = ORIENTED_EDGE ( 'NONE', *, *, #5696, .F. ) ;
#7510 = DIRECTION ( 'NONE',  ( -1.000000000000000000, -0.000000000000000000, -0.000000000000000000 ) ) ;
#7511 = EDGE_CURVE ( 'NONE', #14764, #18692, #6006, .T. ) ;
#7512 = DIRECTION ( 'NONE',  ( -1.000000000000000000, -0.000000000000000000, 0.000000000000000000 ) ) ;
#7513 = CYLINDRICAL_SURFACE ( 'NONE', #6451, 41.00000000000000000 ) ;
#7514 = DIRECTION ( 'NONE',  ( 0.000000000000000000, 0.000000000000000000, 1.000000000000000000 ) ) ;
#7515 = VERTEX_POINT ( 'NONE', #6040 ) ;
#7516 = CARTESIAN_POINT ( 'NONE',  ( -2.250000000000000000, -27.60846790388774608, -2.000000000000000000 ) ) ;
#7517 = CARTESIAN_POINT ( 'NONE',  ( -10.00000000000000000, 0.000000000000000000, 0.000000000000000000 ) ) ;
#7518 = ORIENTED_EDGE ( 'NONE', *, *, #11893, .T. ) ;
#7519 = DIRECTION ( 'NONE',  ( 0.000000000000000000, 0.000000000000000000, 1.000000000000000000 ) ) ;
#7520 = CARTESIAN_POINT ( 'NONE',  ( 11.14999999999999680, 0.000000000000000000, 0.000000000000000000 ) ) ;
#7521 = EDGE_CURVE ( 'NONE', #114, #8902, #11853, .T. ) ;
#7522 = AXIS2_PLACEMENT_3D ( 'NONE', #1522, #10095, #1608 ) ;
#7523 = AXIS2_PLACEMENT_3D ( 'NONE', #1311, #7100, #12923 ) ;
#7524 = AXIS2_PLACEMENT_3D ( 'NONE', #16042, #4076, #9875 ) ;
#7525 = VERTEX_POINT ( 'NONE', #13386 ) ;
#7526 = DIRECTION ( 'NONE',  ( 1.000000000000000000, 0.000000000000000000, 0.000000000000000000 ) ) ;
#7527 = PLANE ( 'NONE',  #6422 ) ;
#7528 = AXIS2_PLACEMENT_3D ( 'NONE', #14355, #11396, #4729 ) ;
#7529 = ORIENTED_EDGE ( 'NONE', *, *, #518, .F. ) ;
#7530 = CARTESIAN_POINT ( 'NONE',  ( -117.1020693116506379, -30.00000000000000000, -17.04080595179801705 ) ) ;
#7531 = CARTESIAN_POINT ( 'NONE',  ( -56.50000000009000445, -34.99999999999999289, 3.817814120399276590E-13 ) ) ;
#7532 = CIRCLE ( 'NONE', #18183, 5.000000000000004441 ) ;
#7533 = PLANE ( 'NONE',  #1774 ) ;
#7534 = DIRECTION ( 'NONE',  ( 1.000000000000000000, 0.000000000000000000, -0.000000000000000000 ) ) ;
#7535 = AXIS2_PLACEMENT_3D ( 'NONE', #16586, #8798, #15942 ) ;
#7536 = LINE ( 'NONE', #7628, #18425 ) ;
#7537 = ORIENTED_EDGE ( 'NONE', *, *, #6437, .F. ) ;
#7538 = CIRCLE ( 'NONE', #870, 7.500000000000007105 ) ;
#7539 = DIRECTION ( 'NONE',  ( -1.000000000000000000, -0.000000000000000000, -0.000000000000000000 ) ) ;
#7540 = EDGE_LOOP ( 'NONE', ( #8158, #16024, #8639, #14458 ) ) ;
#7541 = DIRECTION ( 'NONE',  ( 0.000000000000000000, 0.000000000000000000, 1.000000000000000000 ) ) ;
#7542 = ORIENTED_EDGE ( 'NONE', *, *, #13036, .F. ) ;
#7543 = EDGE_CURVE ( 'NONE', #13366, #15594, #10868, .T. ) ;
#7544 = CONTEXT_DEPENDENT_SHAPE_REPRESENTATION ( #8046, #7856 ) ;
#7545 = ORIENTED_EDGE ( 'NONE', *, *, #18158, .F. ) ;
#7546 = AXIS2_PLACEMENT_3D ( 'NONE', #7954, #13767, #8044 ) ;
#7547 = ORIENTED_EDGE ( 'NONE', *, *, #6549, .T. ) ;
#7548 = VECTOR ( 'NONE', #4311, 1000.000000000000000 ) ;
#7549 = AXIS2_PLACEMENT_3D ( 'NONE', #389, #6194, #11994 ) ;
#7550 = ORIENTED_EDGE ( 'NONE', *, *, #14758, .T. ) ;
#7551 = DIRECTION ( 'NONE',  ( 0.000000000000000000, 0.7071067811865436870, 0.7071067811865513475 ) ) ;
#7552 = DIRECTION ( 'NONE',  ( 0.000000000000000000, 0.000000000000000000, 1.000000000000000000 ) ) ;
#7553 = CYLINDRICAL_SURFACE ( 'NONE', #4823, 63.00000000006298961 ) ;
#7554 = ADVANCED_FACE ( 'NONE', ( #3283 ), #14906, .T. ) ;
#7555 = CYLINDRICAL_SURFACE ( 'NONE', #15221, 56.24900000005625600 ) ;
#7556 = DIRECTION ( 'NONE',  ( 0.000000000000000000, 0.9510565162951520879, 0.3090169943749517811 ) ) ;
#7557 = CIRCLE ( 'NONE', #3016, 24.00000000002399858 ) ;
#7558 = CARTESIAN_POINT ( 'NONE',  ( 0.000000000000000000, 0.000000000000000000, -2.000000000000000000 ) ) ;
#7559 = DIRECTION ( 'NONE',  ( -1.000000000000000000, -0.000000000000000000, -0.000000000000000000 ) ) ;
#7560 = CARTESIAN_POINT ( 'NONE',  ( 0.000000000000000000, 1.178949249685217415, 2.041999999999998483 ) ) ;
#7561 = ORIENTED_EDGE ( 'NONE', *, *, #6249, .T. ) ;
#7562 = AXIS2_PLACEMENT_3D ( 'NONE', #13153, #109, #7519 ) ;
#7563 = EDGE_CURVE ( 'NONE', #9218, #14866, #7826, .T. ) ;
#7564 = CARTESIAN_POINT ( 'NONE',  ( 2.449848172108560096, 3.432307619358740514, -3.503702292528905637 ) ) ;
#7565 = CYLINDRICAL_SURFACE ( 'NONE', #13320, 24.00000000002399858 ) ;
#7566 = AXIS2_PLACEMENT_3D ( 'NONE', #14377, #9897, #1250 ) ;
#7567 = ORIENTED_EDGE ( 'NONE', *, *, #4369, .T. ) ;
#7568 = ORIENTED_EDGE ( 'NONE', *, *, #7485, .T. ) ;
#7569 = CIRCLE ( 'NONE', #12437, 2.649999999999992806 ) ;
#7570 = CARTESIAN_POINT ( 'NONE',  ( -2.000000000000006661, 3.464101615137750834, 0.000000000000000000 ) ) ;
#7571 = CARTESIAN_POINT ( 'NONE',  ( -36.40576474687247099, 15.00000000000001599, 26.45033635316149301 ) ) ;
#7572 = DIRECTION ( 'NONE',  ( 1.000000000000000000, 0.000000000000000000, 0.000000000000000000 ) ) ;
#7573 = VERTEX_POINT ( 'NONE', #9751 ) ;
#7574 = AXIS2_PLACEMENT_3D ( 'NONE', #4041, #18693, #7071 ) ;
#7575 = VECTOR ( 'NONE', #7036, 1000.000000000000000 ) ;
#7576 = CARTESIAN_POINT ( 'NONE',  ( 4.999999999999999112, -13.79392154159179640, 61.47135697633775209 ) ) ;
#7577 = DIRECTION ( 'NONE',  ( 0.000000000000000000, -1.000000000000000000, 0.000000000000000000 ) ) ;
#7578 = CARTESIAN_POINT ( 'NONE',  ( 10.00000000000000000, 27.94286728106393269, 15.73043801031642808 ) ) ;
#7579 = ORIENTED_EDGE ( 'NONE', *, *, #1431, .T. ) ;
#7580 = DIRECTION ( 'NONE',  ( 1.000000000000000000, 0.000000000000000000, 0.000000000000000000 ) ) ;
#7581 = VERTEX_POINT ( 'NONE', #6508 ) ;
#7582 = DIRECTION ( 'NONE',  ( 0.000000000000000000, 0.000000000000000000, -1.000000000000000000 ) ) ;
#7583 = ORIENTED_EDGE ( 'NONE', *, *, #16871, .T. ) ;
#7584 = CARTESIAN_POINT ( 'NONE',  ( 0.000000000000000000, -42.79754323328189969, -11.25576474687263229 ) ) ;
#7585 = CARTESIAN_POINT ( 'NONE',  ( -0.5469614295416921346, 4.303013824936271270, -3.535263753543735454 ) ) ;
#7586 = AXIS2_PLACEMENT_3D ( 'NONE', #14949, #4475, #4658 ) ;
#7587 = ORIENTED_EDGE ( 'NONE', *, *, #8774, .F. ) ;
#7588 = ORIENTED_EDGE ( 'NONE', *, *, #12858, .T. ) ;
#7589 = DIRECTION ( 'NONE',  ( 2.031314180040284764E-16, 1.000000000000000000, 1.301042606982601623E-16 ) ) ;
#7590 = CIRCLE ( 'NONE', #5780, 2.649999999999992806 ) ;
#7591 = ORIENTED_EDGE ( 'NONE', *, *, #6689, .T. ) ;
#7592 = CARTESIAN_POINT ( 'NONE',  ( 10.00000000000000000, 0.000000000000000000, 0.000000000000000000 ) ) ;
#7593 = EDGE_CURVE ( 'NONE', #9087, #9477, #5098, .T. ) ;
#7594 = ADVANCED_FACE ( 'NONE', ( #708, #12705, #2220 ), #18124, .T. ) ;
#7595 = CARTESIAN_POINT ( 'NONE',  ( 4.999999999999999112, 61.03368945066456774, -15.61693798565434044 ) ) ;
#7596 = EDGE_CURVE ( 'NONE', #1279, #18341, #18487, .T. ) ;
#7597 = CIRCLE ( 'NONE', #16434, 4.799999999999999822 ) ;
#7598 = EDGE_LOOP ( 'NONE', ( #15843, #8395, #14802, #4478 ) ) ;
#7599 = VECTOR ( 'NONE', #8145, 1000.000000000000000 ) ;
#7600 = ADVANCED_FACE ( 'NONE', ( #12310 ), #3571, .T. ) ;
#7601 = ORIENTED_EDGE ( 'NONE', *, *, #15532, .T. ) ;
#7602 = CARTESIAN_POINT ( 'NONE',  ( 10.00000000000000000, 46.27827401617404490, 31.97297851452441364 ) ) ;
#7603 = CARTESIAN_POINT ( 'NONE',  ( -0.3562533529037968383, 11.24999999999999467, 23.49729949480461499 ) ) ;
#7604 = DIRECTION ( 'NONE',  ( -1.000000000000000000, 0.000000000000000000, 0.000000000000000000 ) ) ;
#7605 = VERTEX_POINT ( 'NONE', #1085 ) ;
#7607 = DIRECTION ( 'NONE',  ( -1.000000000000000000, 0.000000000000000000, -0.000000000000000000 ) ) ;
#7606 = B_SPLINE_CURVE_WITH_KNOTS ( 'NONE', 3,
 ( #14988, #5693, #2746, #415, #328 ),
 .UNSPECIFIED., .F., .F.,
 ( 4, 1, 4 ),
 ( 0.000000000000000000, 0.002309401076758505790, 0.004618802153517011580 ),
 .UNSPECIFIED. ) ;
#7608 = ADVANCED_FACE ( 'NONE', ( #16605 ), #12414, .F. ) ;
#7609 = CARTESIAN_POINT ( 'NONE',  ( 0.3865131578947368918, -23.49682122285426189, -2.000000000000000000 ) ) ;
#7610 = FACE_BOUND ( 'NONE', #8033, .T. ) ;
#7611 = FACE_BOUND ( 'NONE', #17649, .T. ) ;
#7612 = ORIENTED_EDGE ( 'NONE', *, *, #9203, .F. ) ;
#7613 = FACE_OUTER_BOUND ( 'NONE', #3327, .T. ) ;
#7615 = EDGE_CURVE ( 'NONE', #34, #17821, #2062, .T. ) ;
#7614 = ORIENTED_EDGE ( 'NONE', *, *, #6156, .T. ) ;
#7616 = CARTESIAN_POINT ( 'NONE',  ( 0.000000000000000000, -16.45250512421816680, -53.92768374110909235 ) ) ;
#7617 = DIRECTION ( 'NONE',  ( -0.000000000000000000, -1.000000000000000000, -0.000000000000000000 ) ) ;
#7618 = AXIS2_PLACEMENT_3D ( 'NONE', #9162, #12298, #7728 ) ;
#7619 = EDGE_CURVE ( 'NONE', #12293, #5152, #867, .T. ) ;
#7620 = EDGE_LOOP ( 'NONE', ( #10160, #10331, #10928, #8522 ) ) ;
#7621 = CARTESIAN_POINT ( 'NONE',  ( -0.5000000000000000000, -6.429618962271402616, -1.000000000000000000 ) ) ;
#7622 = VERTEX_POINT ( 'NONE', #16715 ) ;
#7623 = FACE_OUTER_BOUND ( 'NONE', #13499, .T. ) ;
#7624 = EDGE_CURVE ( 'NONE', #8411, #2359, #12401, .T. ) ;
#7625 = LINE ( 'NONE', #17635, #7176 ) ;
#7626 = DIRECTION ( 'NONE',  ( 0.000000000000000000, 0.000000000000000000, 1.000000000000000000 ) ) ;
#7627 = CARTESIAN_POINT ( 'NONE',  ( 13.90576474687263264, 10.00000000000000000, -45.44754323328189827 ) ) ;
#7628 = CARTESIAN_POINT ( 'NONE',  ( -12.69999999999999929, 3.429011037612589670E-15, 28.00000000000000355 ) ) ;
#7629 = ORIENTED_EDGE ( 'NONE', *, *, #8130, .F. ) ;
#7630 = LINE ( 'NONE', #3076, #5764 ) ;
#7631 = ORIENTED_EDGE ( 'NONE', *, *, #9992, .F. ) ;
#7632 = CARTESIAN_POINT ( 'NONE',  ( 0.000000000000000000, 6.799999999999999822, -1.500000000000000000 ) ) ;
#7633 = ORIENTED_EDGE ( 'NONE', *, *, #10060, .T. ) ;
#7634 = ITEM_DEFINED_TRANSFORMATION ( 'NONE', 'NONE', #11086,  #8017 ) ;
#7635 = VERTEX_POINT ( 'NONE', #9652 ) ;
#7636 = CIRCLE ( 'NONE', #12205, 24.00000000002399858 ) ;
#7637 = ORIENTED_EDGE ( 'NONE', *, *, #12616, .T. ) ;
#7638 = EDGE_LOOP ( 'NONE', ( #9546, #16211, #11703, #18435 ) ) ;
#7639 = DIRECTION ( 'NONE',  ( 0.000000000000000000, -0.5877852522924624790, -0.8090169943749551118 ) ) ;
#7640 = DIRECTION ( 'NONE',  ( -1.000000000000000000, 0.000000000000000000, 0.000000000000000000 ) ) ;
#7641 = DIRECTION ( 'NONE',  ( 0.000000000000000000, 0.000000000000000000, 1.000000000000000000 ) ) ;
#7642 = EDGE_CURVE ( 'NONE', #645, #9889, #8455, .T. ) ;
#7643 = DIRECTION ( 'NONE',  ( 0.9995004958639132076, 0.000000000000000000, 0.03160314490350067673 ) ) ;
#7644 = FACE_OUTER_BOUND ( 'NONE', #15257, .T. ) ;
#7645 = DIRECTION ( 'NONE',  ( 0.000000000000000000, 0.000000000000000000, 1.000000000000000000 ) ) ;
#7646 = CARTESIAN_POINT ( 'NONE',  ( 0.6666666666666689611, 4.233901974057261874, -3.300726591567082480 ) ) ;
#7647 = CARTESIAN_POINT ( 'NONE',  ( 0.000000000000000000, -9.514709542736730086, -24.46385708179993301 ) ) ;
#7648 = VERTEX_POINT ( 'NONE', #2131 ) ;
#7649 = DIRECTION ( 'NONE',  ( 0.000000000000000000, 0.000000000000000000, 1.000000000000000000 ) ) ;
#7650 = DIRECTION ( 'NONE',  ( -1.000000000000000000, 0.000000000000000000, 0.000000000000000000 ) ) ;
#7651 = ORIENTED_EDGE ( 'NONE', *, *, #3951, .T. ) ;
#7652 = ORIENTED_EDGE ( 'NONE', *, *, #16675, .T. ) ;
#7653 = CYLINDRICAL_SURFACE ( 'NONE', #1709, 2.649999999999999467 ) ;
#7654 = DIRECTION ( 'NONE',  ( 6.123233995736766036E-17, -1.000000000000000000, 0.000000000000000000 ) ) ;
#7655 = AXIS2_PLACEMENT_3D ( 'NONE', #3073, #8865, #5643 ) ;
#7656 = DIRECTION ( 'NONE',  ( 0.000000000000000000, 0.5877852522924744694, -0.8090169943749464521 ) ) ;
#7657 = ORIENTED_EDGE ( 'NONE', *, *, #6890, .T. ) ;
#7658 = EDGE_CURVE ( 'NONE', #17166, #10426, #16665, .T. ) ;
#7659 = ADVANCED_FACE ( 'NONE', ( #3663 ), #3844, .F. ) ;
#7660 = DIRECTION ( 'NONE',  ( 0.000000000000000000, 0.000000000000000000, 1.000000000000000000 ) ) ;
#7661 = CARTESIAN_POINT ( 'NONE',  ( -0.02448733951239248641, -4.877042772274742255, -3.751161874094027571 ) ) ;
#7662 = CYLINDRICAL_SURFACE ( 'NONE', #3581, 2.649999999999995914 ) ;
#7663 = ORIENTED_EDGE ( 'NONE', *, *, #10152, .F. ) ;
#7664 = CARTESIAN_POINT ( 'NONE',  ( 0.000000000000000000, 0.000000000000000000, 0.000000000000000000 ) ) ;
#7665 = ORIENTED_EDGE ( 'NONE', *, *, #10162, .T. ) ;
#7666 = DIRECTION ( 'NONE',  ( -1.000000000000000000, 0.000000000000000000, 0.000000000000000000 ) ) ;
#7667 = VERTEX_POINT ( 'NONE', #13751 ) ;
#7668 = DIRECTION ( 'NONE',  ( -1.000000000000000000, 0.000000000000000000, 0.000000000000000000 ) ) ;
#7669 = CYLINDRICAL_SURFACE ( 'NONE', #6794, 24.00000000002399503 ) ;
#7670 = ORIENTED_EDGE ( 'NONE', *, *, #15700, .T. ) ;
#7671 = VERTEX_POINT ( 'NONE', #11171 ) ;
#7672 = CARTESIAN_POINT ( 'NONE',  ( -56.50000000009000445, -34.99999999999999289, 3.817814120399276590E-13 ) ) ;
#7673 =( LENGTH_UNIT ( ) NAMED_UNIT ( * ) SI_UNIT ( .MILLI., .METRE. ) );
#7674 = ORIENTED_EDGE ( 'NONE', *, *, #16754, .F. ) ;
#7675 = CARTESIAN_POINT ( 'NONE',  ( 11.25000000000000000, 0.000000000000000000, 0.000000000000000000 ) ) ;
#7676 = AXIS2_PLACEMENT_3D ( 'NONE', #2089, #1887, #4937 ) ;
#7677 = AXIS2_PLACEMENT_3D ( 'NONE', #2641, #15506, #2455 ) ;
#7678 = CIRCLE ( 'NONE', #12563, 12.00000000001200462 ) ;
#7679 = CYLINDRICAL_SURFACE ( 'NONE', #5924, 27.50000000000000000 ) ;
#7680 = ORIENTED_EDGE ( 'NONE', *, *, #13395, .F. ) ;
#7681 = PRODUCT_DEFINITION_SHAPE ( 'NONE', 'NONE',  #18828 ) ;
#7682 = ORIENTED_EDGE ( 'NONE', *, *, #5419, .T. ) ;
#7683 = LINE ( 'NONE', #13509, #10565 ) ;
#7684 = LINE ( 'NONE', #3046, #9573 ) ;
#7685 = CARTESIAN_POINT ( 'NONE',  ( 10.00000000000000000, 40.58063702438398224, -39.14194549634321163 ) ) ;
#7686 = ORIENTED_EDGE ( 'NONE', *, *, #6894, .F. ) ;
#7687 = LINE ( 'NONE', #12077, #4191 ) ;
#7688 = AXIS2_PLACEMENT_3D ( 'NONE', #11193, #17023, #8343 ) ;
#7689 = CARTESIAN_POINT ( 'NONE',  ( 0.000000000000000000, -30.00000000000000000, 0.000000000000000000 ) ) ;
#7690 = CARTESIAN_POINT ( 'NONE',  ( 10.00000000000000000, 9.514709542737238124, -24.46385708179973406 ) ) ;
#7691 = DIRECTION ( 'NONE',  ( -1.000000000000000000, -0.000000000000000000, -0.000000000000000000 ) ) ;
#7692 = ORIENTED_EDGE ( 'NONE', *, *, #725, .T. ) ;
#7693 = VECTOR ( 'NONE', #3239, 1000.000000000000000 ) ;
#7694 = DIRECTION ( 'NONE',  ( -0.000000000000000000, -0.000000000000000000, 1.000000000000000000 ) ) ;
#7695 = ADVANCED_FACE ( 'NONE', ( #6796 ), #8132, .T. ) ;
#7696 = DIRECTION ( 'NONE',  ( -1.000000000000000000, 0.000000000000000000, 0.000000000000000000 ) ) ;
#7697 = EDGE_CURVE ( 'NONE', #3012, #4207, #9459, .T. ) ;
#7698 = ORIENTED_EDGE ( 'NONE', *, *, #9226, .F. ) ;
#7699 = FACE_OUTER_BOUND ( 'NONE', #12000, .T. ) ;
#7700 = DIRECTION ( 'NONE',  ( 0.000000000000000000, -1.224646799147330774E-16, 1.000000000000000000 ) ) ;
#7701 = PRODUCT_DEFINITION_SHAPE ( 'NONE', 'NONE',  #13075 ) ;
#7702 = EDGE_CURVE ( 'NONE', #17281, #179, #5363, .T. ) ;
#7703 = AXIS2_PLACEMENT_3D ( 'NONE', #7843, #7738, #13665 ) ;
#7704 = VERTEX_POINT ( 'NONE', #18696 ) ;
#7705 = DIRECTION ( 'NONE',  ( -1.000000000000000000, 0.000000000000000000, 0.000000000000000000 ) ) ;
#7706 = EDGE_CURVE ( 'NONE', #14393, #14829, #15759, .T. ) ;
#7707 = VERTEX_POINT ( 'NONE', #17457 ) ;
#7708 = CARTESIAN_POINT ( 'NONE',  ( 2.500000000000000000, -1.768423874527823125, 1.021000000000002128 ) ) ;
#7709 = DIRECTION ( 'NONE',  ( -1.000000000000000000, 0.000000000000000000, -0.000000000000000000 ) ) ;
#7710 = CARTESIAN_POINT ( 'NONE',  ( 2.500000000000000000, -2.629050547790028551E-15, -2.041999999999999815 ) ) ;
#7711 = LINE ( 'NONE', #14877, #8576 ) ;
#7712 = CARTESIAN_POINT ( 'NONE',  ( 2.500000000000000000, -1.178949249685213863, 2.042000000000001148 ) ) ;
#7713 = VERTEX_POINT ( 'NONE', #18605 ) ;
#7714 = CYLINDRICAL_SURFACE ( 'NONE', #17031, 24.00000000002399858 ) ;
#7715 = EDGE_LOOP ( 'NONE', ( #18646, #11820, #18119, #13945 ) ) ;
#7716 = ADVANCED_FACE ( 'NONE', ( #15652 ), #7162, .T. ) ;
#7717 = AXIS2_PLACEMENT_3D ( 'NONE', #17283, #5834, #4402 ) ;
#7718 = EDGE_CURVE ( 'NONE', #17227, #4363, #1452, .T. ) ;
#7719 = DIRECTION ( 'NONE',  ( -1.000000000000000000, 0.000000000000000000, -0.000000000000000000 ) ) ;
#7720 = ORIENTED_EDGE ( 'NONE', *, *, #10652, .F. ) ;
#7721 = EDGE_CURVE ( 'NONE', #15269, #13370, #14237, .T. ) ;
#7722 = VERTEX_POINT ( 'NONE', #16027 ) ;
#7723 = EDGE_CURVE ( 'NONE', #607, #10140, #8510, .T. ) ;
#7724 = ORIENTED_EDGE ( 'NONE', *, *, #2447, .T. ) ;
#7725 = ORIENTED_EDGE ( 'NONE', *, *, #13700, .F. ) ;
#7726 = MECHANICAL_DESIGN_GEOMETRIC_PRESENTATION_REPRESENTATION (  '', ( #745 ), #11701 ) ;
#7727 = DIRECTION ( 'NONE',  ( 0.000000000000000000, 0.000000000000000000, 1.000000000000000000 ) ) ;
#7728 = DIRECTION ( 'NONE',  ( 1.000000000000000000, 0.000000000000000000, 0.000000000000000000 ) ) ;
#7729 = DIRECTION ( 'NONE',  ( -0.8191520442889875797, 1.003171929053519570E-16, 0.5735764363510522656 ) ) ;
#7730 = CARTESIAN_POINT ( 'NONE',  ( 32.50000000000000000, -26.50000000000000000, 2.650000000000367617 ) ) ;
#7731 = DIRECTION ( 'NONE',  ( 0.000000000000000000, 0.000000000000000000, 1.000000000000000000 ) ) ;
#7732 = CARTESIAN_POINT ( 'NONE',  ( -0.9999999999999986677, -27.60846790388774608, -2.000000000000000000 ) ) ;
#7733 = FACE_OUTER_BOUND ( 'NONE', #12583, .T. ) ;
#7734 = EDGE_LOOP ( 'NONE', ( #11489, #16 ) ) ;
#7735 = DIRECTION ( 'NONE',  ( 2.220446049250313081E-16, 0.000000000000000000, -1.000000000000000000 ) ) ;
#7736 = ORIENTED_EDGE ( 'NONE', *, *, #12960, .F. ) ;
#7737 = DIRECTION ( 'NONE',  ( -1.000000000000000000, -0.000000000000000000, 0.000000000000000000 ) ) ;
#7738 = DIRECTION ( 'NONE',  ( -1.000000000000000000, 0.000000000000000000, 0.000000000000000000 ) ) ;
#7739 = CARTESIAN_POINT ( 'NONE',  ( 2.500000000000000000, 0.000000000000000000, 0.000000000000000000 ) ) ;
#7740 = ORIENTED_EDGE ( 'NONE', *, *, #18618, .F. ) ;
#7741 = ORIENTED_EDGE ( 'NONE', *, *, #12735, .F. ) ;
#7742 = CARTESIAN_POINT ( 'NONE',  ( -2.855764796983342624, 2.970025579236414082, -0.09382832055445475272 ) ) ;
#7743 = DIRECTION ( 'NONE',  ( 6.123233995736766036E-17, -1.000000000000000000, 0.000000000000000000 ) ) ;
#7744 = AXIS2_PLACEMENT_3D ( 'NONE', #5081, #15197, #17949 ) ;
#7745 = DIRECTION ( 'NONE',  ( 0.000000000000000000, 0.000000000000000000, 1.000000000000000000 ) ) ;
#7746 = EDGE_LOOP ( 'NONE', ( #679, #3362, #15853, #18714 ) ) ;
#7747 = CIRCLE ( 'NONE', #18390, 63.00000000006298961 ) ;
#7748 = AXIS2_PLACEMENT_3D ( 'NONE', #12074, #278, #6169 ) ;
#7749 = EDGE_CURVE ( 'NONE', #4666, #6629, #2598, .T. ) ;
#7750 = CARTESIAN_POINT ( 'NONE',  ( 0.000000000000000000, 0.000000000000000000, 0.000000000000000000 ) ) ;
#7751 = DIRECTION ( 'NONE',  ( 0.000000000000000000, 0.000000000000000000, 1.000000000000000000 ) ) ;
#7752 = CARTESIAN_POINT ( 'NONE',  ( -56.50000000009000445, -34.99999999999999289, 2.650000000000374278 ) ) ;
#7753 = VERTEX_POINT ( 'NONE', #8788 ) ;
#7754 = CARTESIAN_POINT ( 'NONE',  ( 10.00000000000000000, 0.000000000000000000, 0.000000000000000000 ) ) ;
#7755 = AXIS2_PLACEMENT_3D ( 'NONE', #16896, #8030, #18609 ) ;
#7756 = VECTOR ( 'NONE', #13781, 1000.000000000000000 ) ;
#7757 = ORIENTED_EDGE ( 'NONE', *, *, #5088, .F. ) ;
#7758 = DIRECTION ( 'NONE',  ( 0.000000000000000000, 0.000000000000000000, 1.000000000000000000 ) ) ;
#7759 = CIRCLE ( 'NONE', #3819, 56.24900000005625600 ) ;
#7760 = ORIENTED_EDGE ( 'NONE', *, *, #13802, .F. ) ;
#7761 = CARTESIAN_POINT ( 'NONE',  ( 10.00000000000000000, 26.49895292618076326, -49.76630880786279931 ) ) ;
#7762 = CARTESIAN_POINT ( 'NONE',  ( -10.00000000000000000, 0.000000000000000000, 0.000000000000000000 ) ) ;
#7763 = ORIENTED_EDGE ( 'NONE', *, *, #6811, .F. ) ;
#7764 = ORIENTED_EDGE ( 'NONE', *, *, #12092, .F. ) ;
#7765 = CARTESIAN_POINT ( 'NONE',  ( 0.000000000000000000, -2.357898499370432166, 3.035766082959412415E-15 ) ) ;
#7766 =( NAMED_UNIT ( * ) SI_UNIT ( $, .STERADIAN. ) SOLID_ANGLE_UNIT ( ) );
#7767 = EDGE_LOOP ( 'NONE', ( #13784, #4051, #12410, #12605, #9262, #4233, #9103, #6476 ) ) ;
#7768 = DIRECTION ( 'NONE',  ( 0.000000000000000000, -1.000000000000000000, 1.287488025362403787E-15 ) ) ;
#7769 = AXIS2_PLACEMENT_3D ( 'NONE', #8809, #11587, #11294 ) ;
#7770 = AXIS2_PLACEMENT_3D ( 'NONE', #11378, #17198, #4155 ) ;
#7771 = EDGE_CURVE ( 'NONE', #6629, #13789, #7532, .T. ) ;
#7772 = AXIS2_PLACEMENT_3D ( 'NONE', #2429, #13845, #18137 ) ;
#7773 = AXIS2_PLACEMENT_3D ( 'NONE', #10579, #14492, #6009 ) ;
#7774 = CARTESIAN_POINT ( 'NONE',  ( 2.807080416178989513, -3.225969019225150003, -3.502507215260505014 ) ) ;
#7775 = ORIENTED_EDGE ( 'NONE', *, *, #11514, .F. ) ;
#7776 = CIRCLE ( 'NONE', #9006, 24.00000000002399858 ) ;
#7777 = VERTEX_POINT ( 'NONE', #17095 ) ;
#7778 = CARTESIAN_POINT ( 'NONE',  ( -0.3562533529037968383, 11.24999999999999467, 23.49729949480461499 ) ) ;
#7779 = LINE ( 'NONE', #13705, #6829 ) ;
#7781 = AXIS2_PLACEMENT_3D ( 'NONE', #17664, #4610, #10418 ) ;
#7780 = CARTESIAN_POINT ( 'NONE',  ( -4.197393957002303999, -0.8151795401431414234, -3.503767560748935139 ) ) ;
#7782 = ADVANCED_FACE ( 'NONE', ( #15845 ), #5752, .F. ) ;
#7783 = ORIENTED_EDGE ( 'NONE', *, *, #4485, .F. ) ;
#7784 = DIRECTION ( 'NONE',  ( 0.000000000000000000, 0.000000000000000000, 1.000000000000000000 ) ) ;
#7785 = AXIS2_PLACEMENT_3D ( 'NONE', #3942, #2409, #8501 ) ;
#7786 = CARTESIAN_POINT ( 'NONE',  ( 2.687328764639642653, -3.067272167851299969, -0.05923475698271395140 ) ) ;
#7787 = CARTESIAN_POINT ( 'NONE',  ( 10.00000000000000000, -55.33199130079777461, -10.11537145609435306 ) ) ;
#7788 = AXIS2_PLACEMENT_3D ( 'NONE', #4511, #10407, #10491 ) ;
#7789 = LINE ( 'NONE', #9133, #10231 ) ;
#7790 = ORIENTED_EDGE ( 'NONE', *, *, #16216, .F. ) ;
#7791 = AXIS2_PLACEMENT_3D ( 'NONE', #18711, #8437, #1110 ) ;
#7792 = AXIS2_PLACEMENT_3D ( 'NONE', #18670, #18764, #14198 ) ;
#7793 = CARTESIAN_POINT ( 'NONE',  ( 0.000000000000000000, -49.49802920186203892, -26.71881558261783951 ) ) ;
#7794 = EDGE_CURVE ( 'NONE', #9433, #114, #2979, .T. ) ;
#7795 = ORIENTED_EDGE ( 'NONE', *, *, #13017, .F. ) ;
#7796 = CARTESIAN_POINT ( 'NONE',  ( 10.00000000000000000, 22.76987570971527575, 23.88582760061489552 ) ) ;
#7797 = CARTESIAN_POINT ( 'NONE',  ( -79.64793068852898728, -34.99999999999999289, -31.86039329588756530 ) ) ;
#7798 =( REPRESENTATION_RELATIONSHIP ('NONE','NONE', #11014, #8256 ) REPRESENTATION_RELATIONSHIP_WITH_TRANSFORMATION ( #1920 )SHAPE_REPRESENTATION_RELATIONSHIP( ) );
#7799 = AXIS2_PLACEMENT_3D ( 'NONE', #5981, #17697, #1692 ) ;
#7800 = CIRCLE ( 'NONE', #6882, 56.24900000005626310 ) ;
#7801 = AXIS2_PLACEMENT_3D ( 'NONE', #13914, #9899, #15818 ) ;
#7802 = AXIS2_PLACEMENT_3D ( 'NONE', #13699, #8772, #7337 ) ;
#7803 = AXIS2_PLACEMENT_3D ( 'NONE', #11331, #10, #1338 ) ;
#7804 = ORIENTED_EDGE ( 'NONE', *, *, #541, .F. ) ;
#7805 = EDGE_CURVE ( 'NONE', #14399, #17073, #17881, .T. ) ;
#7806 = ORIENTED_EDGE ( 'NONE', *, *, #6214, .F. ) ;
#7807 = SURFACE_STYLE_USAGE ( .BOTH. , #17634 ) ;
#7808 = CARTESIAN_POINT ( 'NONE',  ( -11.25000000000000355, 0.000000000000000000, 0.000000000000000000 ) ) ;
#7809 = CARTESIAN_POINT ( 'NONE',  ( 0.000000000000000000, 11.24999999999999467, 0.000000000000000000 ) ) ;
#7810 = AXIS2_PLACEMENT_3D ( 'NONE', #11801, #17608, #3223 ) ;
#7811 = CARTESIAN_POINT ( 'NONE',  ( 0.2500000000000002220, 4.898587196589412829E-16, -4.000000000000000000 ) ) ;
#7812 = EDGE_LOOP ( 'NONE', ( #16998, #4735, #3648, #11585, #14496, #5454, #3027, #8585, #1210, #12326, #4681, #2061, #161, #722, #5527, #6775 ) ) ;
#7813 = DIRECTION ( 'NONE',  ( -1.000000000000000000, -0.000000000000000000, -0.000000000000000000 ) ) ;
#7814 = AXIS2_PLACEMENT_3D ( 'NONE', #10929, #3703, #14277 ) ;
#7815 = CARTESIAN_POINT ( 'NONE',  ( 5.000000000000000000, -48.50907078259410099, 40.19788616105593348 ) ) ;
#7816 = ORIENTED_EDGE ( 'NONE', *, *, #2491, .T. ) ;
#7817 = AXIS2_PLACEMENT_3D ( 'NONE', #6822, #8062, #940 ) ;
#7818 = VECTOR ( 'NONE', #16595, 1000.000000000000000 ) ;
#7819 = ITEM_DEFINED_TRANSFORMATION ( 'NONE', 'NONE', #10471,  #8017 ) ;
#7820 = ORIENTED_EDGE ( 'NONE', *, *, #18368, .F. ) ;
#7821 = ORIENTED_EDGE ( 'NONE', *, *, #13156, .T. ) ;
#7822 = TOROIDAL_SURFACE ( 'NONE', #2371, 29.90000000000000213, 0.1000000000000028644 ) ;
#7823 = EDGE_CURVE ( 'NONE', #11271, #13113, #16384, .T. ) ;
#7824 = ADVANCED_FACE ( 'NONE', ( #15933 ), #37, .T. ) ;
#7825 = ORIENTED_EDGE ( 'NONE', *, *, #11679, .T. ) ;
#7826 = CIRCLE ( 'NONE', #6929, 2.649999999999999467 ) ;
#7827 = DIRECTION ( 'NONE',  ( -1.000000000000000000, 0.000000000000000000, 0.000000000000000000 ) ) ;
#7828 = ADVANCED_FACE ( 'NONE', ( #1188 ), #4403, .F. ) ;
#7829 = CARTESIAN_POINT ( 'NONE',  ( 10.00000000000000000, 6.799999999999999822, 0.000000000000000000 ) ) ;
#7830 = AXIS2_PLACEMENT_3D ( 'NONE', #11391, #17211, #9969 ) ;
#7831 = AXIS2_PLACEMENT_3D ( 'NONE', #5828, #4224, #8864 ) ;
#7832 = PLANE ( 'NONE',  #1471 ) ;
#7833 = CARTESIAN_POINT ( 'NONE',  ( -26.29305231718568336, -26.50000000000000000, -19.10302069950552095 ) ) ;
#7834 = CARTESIAN_POINT ( 'NONE',  ( 0.000000000000000000, 0.000000000000000000, 0.000000000000000000 ) ) ;
#7835 = ADVANCED_FACE ( 'NONE', ( #14410 ), #7350, .T. ) ;
#7836 = DIRECTION ( 'NONE',  ( -1.000000000000000000, -0.000000000000000000, -0.000000000000000000 ) ) ;
#7837 = CARTESIAN_POINT ( 'NONE',  ( 10.00000000000000000, -25.42247726998023083, 12.18267823974742470 ) ) ;
#7838 = CYLINDRICAL_SURFACE ( 'NONE', #11106, 24.00000000002399503 ) ;
#7839 = ORIENTED_EDGE ( 'NONE', *, *, #6682, .T. ) ;
#7840 = FACE_OUTER_BOUND ( 'NONE', #14199, .T. ) ;
#7841 = ORIENTED_EDGE ( 'NONE', *, *, #562, .T. ) ;
#7842 = DIRECTION ( 'NONE',  ( 0.000000000000000000, 0.000000000000000000, 1.000000000000000000 ) ) ;
#7843 = CARTESIAN_POINT ( 'NONE',  ( 10.00000000000000000, 0.000000000000000000, 0.000000000000000000 ) ) ;
#7844 = DIRECTION ( 'NONE',  ( -1.000000000000000000, 0.000000000000000000, 0.000000000000000000 ) ) ;
#7845 = AXIS2_PLACEMENT_3D ( 'NONE', #1378, #12816, #12719 ) ;
#7846 = ORIENTED_EDGE ( 'NONE', *, *, #14359, .T. ) ;
#7847 = VERTEX_POINT ( 'NONE', #17373 ) ;
#7848 = FACE_OUTER_BOUND ( 'NONE', #5415, .T. ) ;
#7849 = DIRECTION ( 'NONE',  ( 0.000000000000000000, 0.000000000000000000, 1.000000000000000000 ) ) ;
#7850 = VECTOR ( 'NONE', #12002, 1000.000000000000000 ) ;
#7851 = EDGE_CURVE ( 'NONE', #9159, #16839, #8688, .T. ) ;
#7852 = DIRECTION ( 'NONE',  ( -1.000000000000000000, 0.000000000000000000, 0.000000000000000000 ) ) ;
#7853 = ORIENTED_EDGE ( 'NONE', *, *, #8548, .F. ) ;
#7854 = CIRCLE ( 'NONE', #18500, 56.24900000005625600 ) ;
#7855 = AXIS2_PLACEMENT_3D ( 'NONE', #11621, #5718, #1340 ) ;
#7856 = PRODUCT_DEFINITION_SHAPE ( 'NONE', 'NONE',  #18825 ) ;
#7857 = EDGE_CURVE ( 'NONE', #3893, #9406, #11520, .T. ) ;
#7858 = DIRECTION ( 'NONE',  ( -1.000000000000000000, -0.000000000000000000, -0.000000000000000000 ) ) ;
#7859 = DIRECTION ( 'NONE',  ( 2.220446049250313081E-16, 0.000000000000000000, 1.000000000000000000 ) ) ;
#7860 = CIRCLE ( 'NONE', #14865, 20.00000000000000000 ) ;
#7861 = CARTESIAN_POINT ( 'NONE',  ( 0.000000000000000000, 0.000000000000000000, -1.000000000000000000 ) ) ;
#7862 = ORIENTED_EDGE ( 'NONE', *, *, #13301, .T. ) ;
#7863 = LINE ( 'NONE', #15206, #9777 ) ;
#7864 = CIRCLE ( 'NONE', #10299, 2.649999999999992806 ) ;
#7865 = VECTOR ( 'NONE', #18111, 1000.000000000000000 ) ;
#7866 = VERTEX_POINT ( 'NONE', #1635 ) ;
#7867 = AXIS2_PLACEMENT_3D ( 'NONE', #12181, #10455, #14745 ) ;
#7868 = CARTESIAN_POINT ( 'NONE',  ( 0.000000000000000000, 4.769696007084728073, -1.500000000000000000 ) ) ;
#7869 = VERTEX_POINT ( 'NONE', #17921 ) ;
#7870 = EDGE_CURVE ( 'NONE', #18131, #10711, #7238, .T. ) ;
#7871 = DIRECTION ( 'NONE',  ( -1.000000000000000000, 0.000000000000000000, 0.000000000000000000 ) ) ;
#7872 = DIRECTION ( 'NONE',  ( 0.000000000000000000, 0.000000000000000000, 1.000000000000000000 ) ) ;
#7873 = ORIENTED_EDGE ( 'NONE', *, *, #16567, .F. ) ;
#7874 = ORIENTED_EDGE ( 'NONE', *, *, #1771, .T. ) ;
#7875 = CARTESIAN_POINT ( 'NONE',  ( 10.00000000000000000, 53.92768374110868734, 16.45250512421953459 ) ) ;
#7876 = VERTEX_POINT ( 'NONE', #9154 ) ;
#7877 = CARTESIAN_POINT ( 'NONE',  ( 5.000000000000000000, 33.71303790549352186, -53.22058882792159551 ) ) ;
#7878 = VECTOR ( 'NONE', #17642, 1000.000000000000000 ) ;
#7879 = AXIS2_PLACEMENT_3D ( 'NONE', #8469, #1325, #9707 ) ;
#7880 = AXIS2_PLACEMENT_3D ( 'NONE', #11690, #17494, #1137 ) ;
#7881 = DIRECTION ( 'NONE',  ( 0.000000000000000000, 0.8090169943749486725, -0.5877852522924713607 ) ) ;
#7882 = CARTESIAN_POINT ( 'NONE',  ( 0.000000000000000000, 0.000000000000000000, 3.469446951953614189E-15 ) ) ;
#7883 = ORIENTED_EDGE ( 'NONE', *, *, #16129, .F. ) ;
#7884 = AXIS2_PLACEMENT_3D ( 'NONE', #8936, #4383, #17794 ) ;
#7885 = ORIENTED_EDGE ( 'NONE', *, *, #3262, .F. ) ;
#7886 = DIRECTION ( 'NONE',  ( -1.000000000000000000, -0.000000000000000000, -0.000000000000000000 ) ) ;
#7887 = DIRECTION ( 'NONE',  ( -0.01515971714484241201, 0.000000000000000000, 0.9998850848853023665 ) ) ;
#7888 = CARTESIAN_POINT ( 'NONE',  ( 0.000000000000000000, -19.44239304137360946, -20.41355805489636310 ) ) ;
#7889 = ORIENTED_EDGE ( 'NONE', *, *, #15039, .F. ) ;
#7890 = CARTESIAN_POINT ( 'NONE',  ( 2.100000000000000089, 0.000000000000000000, -0.2800830152838844622 ) ) ;
#7891 = ADVANCED_FACE ( 'NONE', ( #10400 ), #3080, .F. ) ;
#7892 = CIRCLE ( 'NONE', #3952, 24.00000000002399858 ) ;
#7893 = CARTESIAN_POINT ( 'NONE',  ( 3.355112389629172576, -2.681727112203168950, -0.2256878752776777242 ) ) ;
#7894 = DIRECTION ( 'NONE',  ( 0.000000000000000000, 0.4999999999999991118, -0.8660254037844391517 ) ) ;
#7895 = CARTESIAN_POINT ( 'NONE',  ( -31.74999999999995737, 0.000000000000000000, 0.000000000000000000 ) ) ;
#7896 = ORIENTED_EDGE ( 'NONE', *, *, #5858, .T. ) ;
#7897 = CARTESIAN_POINT ( 'NONE',  ( 10.00000000000000000, 13.40641754777665717, 24.79895094899264052 ) ) ;
#7898 = ORIENTED_EDGE ( 'NONE', *, *, #15276, .F. ) ;
#7899 = CARTESIAN_POINT ( 'NONE',  ( -10.00000000000000000, -42.79754323328189969, -13.90576474687263264 ) ) ;
#7900 = CARTESIAN_POINT ( 'NONE',  ( 0.000000000000000000, 16.45250512421856470, 53.92768374110897156 ) ) ;
#7901 = AXIS2_PLACEMENT_3D ( 'NONE', #12874, #4297, #10100 ) ;
#7902 = CIRCLE ( 'NONE', #13094, 12.00000000001200107 ) ;
#7903 = ADVANCED_FACE ( 'NONE', ( #16212 ), #8957, .T. ) ;
#7904 = VERTEX_POINT ( 'NONE', #7439 ) ;
#7905 = EDGE_CURVE ( 'NONE', #10656, #6965, #14974, .T. ) ;
#7906 = ORIENTED_EDGE ( 'NONE', *, *, #7593, .T. ) ;
#7907 = CARTESIAN_POINT ( 'NONE',  ( 4.197478902586992966, -0.8524102783748346290, -3.505063281295504041 ) ) ;
#7908 = CARTESIAN_POINT ( 'NONE',  ( 0.000000000000000000, 19.44239304137375868, 20.41355805489622455 ) ) ;
#7909 = DIRECTION ( 'NONE',  ( -0.000000000000000000, -0.000000000000000000, 1.000000000000000000 ) ) ;
#7910 = DIRECTION ( 'NONE',  ( 0.000000000000000000, 0.000000000000000000, 1.000000000000000000 ) ) ;
#7911 = CARTESIAN_POINT ( 'NONE',  ( 10.00000000000000000, 25.38428207620322752, 6.681932690257054830 ) ) ;
#7912 = ORIENTED_EDGE ( 'NONE', *, *, #11214, .T. ) ;
#7914 = DIRECTION ( 'NONE',  ( -1.000000000000000000, 0.000000000000000000, 0.000000000000000000 ) ) ;
#7913 = CIRCLE ( 'NONE', #4572, 2.649999999999992806 ) ;
#7915 = AXIS2_PLACEMENT_3D ( 'NONE', #5160, #18215, #16789 ) ;
#7916 = CARTESIAN_POINT ( 'NONE',  ( -4.000000000000000000, -2.309401076758515803, -0.4999999999999995559 ) ) ;
#7917 = VERTEX_POINT ( 'NONE', #3163 ) ;
#7918 = ITEM_DEFINED_TRANSFORMATION ( 'NONE', 'NONE', #15343,  #8017 ) ;
#7919 = ORIENTED_EDGE ( 'NONE', *, *, #11923, .F. ) ;
#7920 = ORIENTED_EDGE ( 'NONE', *, *, #10297, .F. ) ;
#7921 = ORIENTED_EDGE ( 'NONE', *, *, #9117, .F. ) ;
#7922 = AXIS2_PLACEMENT_3D ( 'NONE', #17444, #14583, #5737 ) ;
#7923 = CARTESIAN_POINT ( 'NONE',  ( 0.000000000000000000, 13.24999999999999822, 0.000000000000000000 ) ) ;
#7924 = DIRECTION ( 'NONE',  ( 1.000000000000000000, 0.000000000000000000, 0.000000000000000000 ) ) ;
#7925 = DIRECTION ( 'NONE',  ( 0.000000000000000000, 0.000000000000000000, 1.000000000000000000 ) ) ;
#7926 = SURFACE_STYLE_FILL_AREA ( #4968 ) ;
#7927 = LINE ( 'NONE', #9451, #1169 ) ;
#7928 = DIRECTION ( 'NONE',  ( 0.9899144417285629105, 0.000000000000000000, -0.1416665029469836301 ) ) ;
#7929 = CARTESIAN_POINT ( 'NONE',  ( 0.000000000000000000, 2.357898499370431722, -2.818925648462311528E-15 ) ) ;
#7930 = ORIENTED_EDGE ( 'NONE', *, *, #18573, .F. ) ;
#7931 = CARTESIAN_POINT ( 'NONE',  ( 0.000000000000000000, -4.381479206523217762, 32.70783759231085241 ) ) ;
#7932 = VERTEX_POINT ( 'NONE', #11737 ) ;
#7933 = CARTESIAN_POINT ( 'NONE',  ( 10.00000000000000000, -53.22058882792171630, -33.71303790549333712 ) ) ;
#7934 = DIRECTION ( 'NONE',  ( 0.000000000000000000, 0.000000000000000000, -1.000000000000000000 ) ) ;
#7935 = ORIENTED_EDGE ( 'NONE', *, *, #4365, .F. ) ;
#7936 = ORIENTED_EDGE ( 'NONE', *, *, #14244, .T. ) ;
#7937 = EDGE_CURVE ( 'NONE', #11956, #7161, #10658, .T. ) ;
#7938 = DIRECTION ( 'NONE',  ( -0.000000000000000000, 1.000000000000000000, -0.000000000000000000 ) ) ;
#7939 = CIRCLE ( 'NONE', #7336, 27.29487558977753991 ) ;
#7940 = CARTESIAN_POINT ( 'NONE',  ( -90.00000000009001155, -1.688217584298307050E-14, 4.933119884809045175E-15 ) ) ;
#7942 = EDGE_CURVE ( 'NONE', #9997, #8150, #6949, .T. ) ;
#7941 = CARTESIAN_POINT ( 'NONE',  ( -3.511755186886750479, 2.826662030176366081, -3.597382984111578086 ) ) ;
#7943 = ORIENTED_EDGE ( 'NONE', *, *, #5867, .F. ) ;
#7944 = EDGE_CURVE ( 'NONE', #8606, #12076, #13041, .T. ) ;
#7945 = EDGE_CURVE ( 'NONE', #13284, #10808, #6202, .T. ) ;
#7946 = DIRECTION ( 'NONE',  ( 0.000000000000000000, 1.000000000000000000, 0.000000000000000000 ) ) ;
#7947 = FACE_BOUND ( 'NONE', #4985, .T. ) ;
#7948 = DIRECTION ( 'NONE',  ( -1.000000000000000000, 0.000000000000000000, 0.000000000000000000 ) ) ;
#7949 = ORIENTED_EDGE ( 'NONE', *, *, #5967, .T. ) ;
#7951 = DIRECTION ( 'NONE',  ( -1.000000000000000000, 0.000000000000000000, 0.000000000000000000 ) ) ;
#7950 = VECTOR ( 'NONE', #8611, 1000.000000000000000 ) ;
#7952 = EDGE_CURVE ( 'NONE', #18552, #16201, #9753, .T. ) ;
#7953 = ORIENTED_EDGE ( 'NONE', *, *, #11072, .F. ) ;
#7954 = CARTESIAN_POINT ( 'NONE',  ( 0.000000000000000000, 9.823366686501460165, -55.51919907100641893 ) ) ;
#7955 = ORIENTED_EDGE ( 'NONE', *, *, #13718, .F. ) ;
#7956 = AXIS2_PLACEMENT_3D ( 'NONE', #9238, #14768, #1822 ) ;
#7957 = DIRECTION ( 'NONE',  ( 1.000000000000000000, 0.000000000000000000, 0.000000000000000000 ) ) ;
#7958 = AXIS2_PLACEMENT_3D ( 'NONE', #3906, #2468, #8283 ) ;
#7959 = CARTESIAN_POINT ( 'NONE',  ( 10.00000000000000000, 1.017308535512385870, 56.37237871411034007 ) ) ;
#7960 = ORIENTED_EDGE ( 'NONE', *, *, #2377, .F. ) ;
#7961 = ORIENTED_EDGE ( 'NONE', *, *, #18337, .T. ) ;
#7962 = EDGE_CURVE ( 'NONE', #5427, #17735, #18498, .T. ) ;
#7963 = DIRECTION ( 'NONE',  ( -1.000000000000000000, -0.000000000000000000, 0.000000000000000000 ) ) ;
#7964 = FILL_AREA_STYLE_COLOUR ( '', #13210 ) ;
#7965 = EDGE_CURVE ( 'NONE', #2359, #13122, #12420, .T. ) ;
#7966 = ORIENTED_EDGE ( 'NONE', *, *, #5200, .F. ) ;
#7967 = CARTESIAN_POINT ( 'NONE',  ( 10.00000000000000000, 29.75305054077492173, -14.27431201565494412 ) ) ;
#7968 = ADVANCED_FACE ( 'NONE', ( #1917 ), #17549, .T. ) ;
#7969 = ADVANCED_FACE ( 'NONE', ( #6297 ), #13542, .F. ) ;
#7970 = CIRCLE ( 'NONE', #18621, 2.649999999999985700 ) ;
#7971 = DIRECTION ( 'NONE',  ( 0.000000000000000000, 0.000000000000000000, 1.000000000000000000 ) ) ;
#7972 = DIRECTION ( 'NONE',  ( 0.000000000000000000, 0.000000000000000000, 1.000000000000000000 ) ) ;
#7973 = ORIENTED_EDGE ( 'NONE', *, *, #10936, .F. ) ;
#7974 = VERTEX_POINT ( 'NONE', #7632 ) ;
#7975 = CARTESIAN_POINT ( 'NONE',  ( 0.000000000000000000, 22.76987570971527575, 23.88582760061489552 ) ) ;
#7976 = DIRECTION ( 'NONE',  ( 0.000000000000000000, 0.000000000000000000, -1.000000000000000000 ) ) ;
#7977 = DIRECTION ( 'NONE',  ( -1.000000000000000000, 0.000000000000000000, 0.000000000000000000 ) ) ;
#7978 = VERTEX_POINT ( 'NONE', #15063 ) ;
#7979 = FACE_OUTER_BOUND ( 'NONE', #14626, .T. ) ;
#7980 = DIRECTION ( 'NONE',  ( 1.000000000000000000, 0.000000000000000000, 0.000000000000000000 ) ) ;
#7981 = CARTESIAN_POINT ( 'NONE',  ( -10.00000000000000000, 0.000000000000000000, 0.000000000000000000 ) ) ;
#7982 = CYLINDRICAL_SURFACE ( 'NONE', #6275, 2.500000000000000444 ) ;
#7983 = ORIENTED_EDGE ( 'NONE', *, *, #6706, .F. ) ;
#7984 = DIRECTION ( 'NONE',  ( 0.000000000000000000, -0.9510565162951565288, 0.3090169943749384029 ) ) ;
#7985 = AXIS2_PLACEMENT_3D ( 'NONE', #6270, #13794, #756 ) ;
#7986 = ORIENTED_EDGE ( 'NONE', *, *, #13791, .T. ) ;
#7987 = DIRECTION ( 'NONE',  ( 0.000000000000000000, 1.000000000000000000, 3.491481338843133355E-15 ) ) ;
#7988 = CIRCLE ( 'NONE', #17125, 2.649999999999992806 ) ;
#7989 = CARTESIAN_POINT ( 'NONE',  ( 0.000000000000000000, 42.79754323328179311, -13.90576474687299680 ) ) ;
#7990 = EDGE_CURVE ( 'NONE', #15870, #9667, #2688, .T. ) ;
#7991 = ORIENTED_EDGE ( 'NONE', *, *, #18603, .T. ) ;
#7992 = AXIS2_PLACEMENT_3D ( 'NONE', #15384, #8155, #13967 ) ;
#7993 = ORIENTED_EDGE ( 'NONE', *, *, #1787, .F. ) ;
#7994 = DIRECTION ( 'NONE',  ( 0.000000000000000000, 0.000000000000000000, 1.000000000000000000 ) ) ;
#7995 = VECTOR ( 'NONE', #14306, 1000.000000000000000 ) ;
#7996 = CARTESIAN_POINT ( 'NONE',  ( 3.999999999999999112, -0.3979232138631231819, -5.929230630780099908E-17 ) ) ;
#7997 = CYLINDRICAL_SURFACE ( 'NONE', #15123, 12.00000000001200462 ) ;
#7998 = DIRECTION ( 'NONE',  ( 0.000000000000000000, 0.000000000000000000, 1.000000000000000000 ) ) ;
#7999 = DIRECTION ( 'NONE',  ( -1.000000000000000000, -0.000000000000000000, -0.000000000000000000 ) ) ;
#8000 = DIRECTION ( 'NONE',  ( 0.000000000000000000, -0.4539904997395350916, -0.8910065241883737830 ) ) ;
#8001 = VERTEX_POINT ( 'NONE', #12580 ) ;
#8002 = CARTESIAN_POINT ( 'NONE',  ( -4.235886605889389145, -2.417314728048544303, -3.751161874094020909 ) ) ;
#8003 = ADVANCED_FACE ( 'NONE', ( #3820 ), #9623, .T. ) ;
#8004 =( LENGTH_UNIT ( ) NAMED_UNIT ( * ) SI_UNIT ( .MILLI., .METRE. ) );
#8005 = DIRECTION ( 'NONE',  ( -1.000000000000000000, -0.000000000000000000, 0.000000000000000000 ) ) ;
#8006 = ORIENTED_EDGE ( 'NONE', *, *, #6682, .F. ) ;
#8007 = ITEM_DEFINED_TRANSFORMATION ( 'NONE', 'NONE', #3515,  #8017 ) ;
#8008 = EDGE_CURVE ( 'NONE', #8632, #11858, #13731, .T. ) ;
#8009 = AXIS2_PLACEMENT_3D ( 'NONE', #15775, #9958, #8707 ) ;
#8010 = VERTEX_POINT ( 'NONE', #15445 ) ;
#8011 = ORIENTED_EDGE ( 'NONE', *, *, #3824, .T. ) ;
#8012 = VERTEX_POINT ( 'NONE', #974 ) ;
#8013 = DIRECTION ( 'NONE',  ( -1.000000000000000000, -0.000000000000000000, -0.000000000000000000 ) ) ;
#8014 = DIRECTION ( 'NONE',  ( 0.000000000000000000, 0.000000000000000000, -1.000000000000000000 ) ) ;
#8015 = CARTESIAN_POINT ( 'NONE',  ( 10.00000000000000000, 0.000000000000000000, 0.000000000000000000 ) ) ;
#8016 = CARTESIAN_POINT ( 'NONE',  ( 32.50000000000000000, -30.00000000000000000, -2.649999999999631317 ) ) ;
#8017 = AXIS2_PLACEMENT_3D ( 'NONE', #12801, #14324, #9934 ) ;
#8018 = CARTESIAN_POINT ( 'NONE',  ( 10.00000000000000000, -26.71881558261695133, -49.49802920186252209 ) ) ;
#8019 = CARTESIAN_POINT ( 'NONE',  ( 2.000000000000005329, -3.464101615137751722, 0.000000000000000000 ) ) ;
#8020 = CARTESIAN_POINT ( 'NONE',  ( 0.000000000000000000, -31.97297851452390915, -46.27827401617439307 ) ) ;
#8021 = VERTEX_POINT ( 'NONE', #4959 ) ;
#8022 = DIRECTION ( 'NONE',  ( 0.000000000000000000, 0.7071067811865486830, -0.7071067811865463515 ) ) ;
#8023 = VERTEX_POINT ( 'NONE', #13814 ) ;
#8024 = EDGE_CURVE ( 'NONE', #139, #13167, #9527, .T. ) ;
#8025 = DIRECTION ( 'NONE',  ( -1.000000000000000000, -0.000000000000000000, -0.000000000000000000 ) ) ;
#8026 = CARTESIAN_POINT ( 'NONE',  ( 5.000000000000000888, 0.000000000000000000, 0.000000000000000000 ) ) ;
#8027 = ORIENTED_EDGE ( 'NONE', *, *, #7281, .T. ) ;
#8028 = ORIENTED_EDGE ( 'NONE', *, *, #3757, .F. ) ;
#8029 = DIRECTION ( 'NONE',  ( 0.000000000000000000, 0.000000000000000000, 1.000000000000000000 ) ) ;
#8030 = DIRECTION ( 'NONE',  ( -8.173385717056413707E-17, -1.000000000000000000, -1.077247711435613592E-16 ) ) ;
#8031 = ADVANCED_FACE ( 'NONE', ( #9336 ), #3641, .F. ) ;
#8032 = DIRECTION ( 'NONE',  ( 0.000000000000000000, 0.000000000000000000, 1.000000000000000000 ) ) ;
#8033 = EDGE_LOOP ( 'NONE', ( #15335, #8823 ) ) ;
#8034 = COLOUR_RGB ( '',1.000000000000000000, 0.9490196078431372140, 0.9098039215686274384 ) ;
#8035 = CARTESIAN_POINT ( 'NONE',  ( -117.1020693116506379, -30.00000000000000000, -19.69080595179801207 ) ) ;
#8036 = LINE ( 'NONE', #16527, #12474 ) ;
#8037 = DIRECTION ( 'NONE',  ( 0.000000000000000000, 0.000000000000000000, 1.000000000000000000 ) ) ;
#8038 = ORIENTED_EDGE ( 'NONE', *, *, #14776, .F. ) ;
#8039 = EDGE_CURVE ( 'NONE', #9028, #5885, #10287, .T. ) ;
#8040 = DIRECTION ( 'NONE',  ( -0.000000000000000000, -0.000000000000000000, -1.000000000000000000 ) ) ;
#8041 = EDGE_CURVE ( 'NONE', #16577, #7464, #4805, .T. ) ;
#8042 = ORIENTED_EDGE ( 'NONE', *, *, #17293, .T. ) ;
#8043 = UNCERTAINTY_MEASURE_WITH_UNIT (LENGTH_MEASURE( 1.000000000000000082E-05 ), #1180, 'distance_accuracy_value', 'NONE');
#8044 = DIRECTION ( 'NONE',  ( 0.000000000000000000, -0.8090169943749402348, -0.5877852522924830181 ) ) ;
#8045 = ORIENTED_EDGE ( 'NONE', *, *, #2535, .T. ) ;
#8046 =( REPRESENTATION_RELATIONSHIP ('NONE','NONE', #11014, #8256 ) REPRESENTATION_RELATIONSHIP_WITH_TRANSFORMATION ( #7634 )SHAPE_REPRESENTATION_RELATIONSHIP( ) );
#8047 = PRODUCT_DEFINITION ( 'UNKNOWN', '', #16897, #2541 ) ;
#8048 = LINE ( 'NONE', #9286, #7178 ) ;
#8049 = CYLINDRICAL_SURFACE ( 'NONE', #10137, 24.00000000002399858 ) ;
#8050 = DIRECTION ( 'NONE',  ( 0.000000000000000000, 0.000000000000000000, -1.000000000000000000 ) ) ;
#8051 = ORIENTED_EDGE ( 'NONE', *, *, #18511, .F. ) ;
#8052 = ORIENTED_EDGE ( 'NONE', *, *, #6440, .T. ) ;
#8053 = AXIS2_PLACEMENT_3D ( 'NONE', #12459, #18265, #5119 ) ;
#8054 = CARTESIAN_POINT ( 'NONE',  ( 0.000000000000000000, 11.24999999999999467, 0.000000000000000000 ) ) ;
#8055 = APPLICATION_PROTOCOL_DEFINITION ( 'draft international standard', 'automotive_design', 1998, #10463 ) ;
#8056 = ORIENTED_EDGE ( 'NONE', *, *, #5110, .F. ) ;
#8057 = CARTESIAN_POINT ( 'NONE',  ( -117.1020693116508085, -38.00000000000000000, 17.04080595179778967 ) ) ;
#8058 = B_SPLINE_CURVE_WITH_KNOTS ( 'NONE', 3,
 ( #9567, #15383, #926, #6812, #10805, #16823, #16627, #3685 ),
 .UNSPECIFIED., .F., .F.,
 ( 4, 2, 2, 4 ),
 ( 2.465131517075058656E-07, 0.001183067374689851080, 0.001774477805458923299, 0.002365888236227995517 ),
 .UNSPECIFIED. ) ;
#8059 = VECTOR ( 'NONE', #12753, 1000.000000000000000 ) ;
#8060 = DIRECTION ( 'NONE',  ( 0.000000000000000000, 0.000000000000000000, -1.000000000000000000 ) ) ;
#8061 = AXIS2_PLACEMENT_3D ( 'NONE', #16641, #650, #6452 ) ;
#8063 = AXIS2_PLACEMENT_3D ( 'NONE', #11557, #14404, #4127 ) ;
#8062 = DIRECTION ( 'NONE',  ( -0.000000000000000000, 1.000000000000000000, -0.000000000000000000 ) ) ;
#8064 = ORIENTED_EDGE ( 'NONE', *, *, #7474, .T. ) ;
#8065 = EDGE_CURVE ( 'NONE', #4831, #3895, #13949, .T. ) ;
#8066 = CARTESIAN_POINT ( 'NONE',  ( 10.00000000000000000, -42.79754323328189969, -16.55576474687263300 ) ) ;
#8067 = EDGE_CURVE ( 'NONE', #4436, #10666, #2287, .T. ) ;
#8068 = EDGE_CURVE ( 'NONE', #4319, #7125, #8106, .T. ) ;
#8069 = ORIENTED_EDGE ( 'NONE', *, *, #18302, .F. ) ;
#8070 = DIRECTION ( 'NONE',  ( 0.000000000000000000, -0.000000000000000000, 1.000000000000000000 ) ) ;
#8071 = DIRECTION ( 'NONE',  ( 0.000000000000000000, 0.000000000000000000, 1.000000000000000000 ) ) ;
#8072 = DIRECTION ( 'NONE',  ( 1.000000000000000000, 0.000000000000000000, 0.000000000000000000 ) ) ;
#8073 = ORIENTED_EDGE ( 'NONE', *, *, #13595, .F. ) ;
#8074 = DIRECTION ( 'NONE',  ( -2.031314180040284764E-16, -1.000000000000000000, -1.301042606982601377E-16 ) ) ;
#8075 = ORIENTED_EDGE ( 'NONE', *, *, #578, .T. ) ;
#8076 = EDGE_CURVE ( 'NONE', #7978, #1162, #8166, .T. ) ;
#8077 = DIRECTION ( 'NONE',  ( 0.000000000000000000, 0.000000000000000000, 1.000000000000000000 ) ) ;
#8078 = CYLINDRICAL_SURFACE ( 'NONE', #14380, 63.00000000006298961 ) ;
#8079 = VECTOR ( 'NONE', #15889, 1000.000000000000000 ) ;
#8080 = ORIENTED_EDGE ( 'NONE', *, *, #13975, .F. ) ;
#8081 = EDGE_LOOP ( 'NONE', ( #14207, #14077, #7961, #3395 ) ) ;
#8082 = CARTESIAN_POINT ( 'NONE',  ( 10.00000000000000000, 0.000000000000000000, 0.000000000000000000 ) ) ;
#8083 = ORIENTED_EDGE ( 'NONE', *, *, #11068, .F. ) ;
#8084 = DIRECTION ( 'NONE',  ( -1.000000000000000000, 0.000000000000000000, -0.000000000000000000 ) ) ;
#8085 = DIRECTION ( 'NONE',  ( -0.000000000000000000, 1.000000000000000000, -0.000000000000000000 ) ) ;
#8086 = CIRCLE ( 'NONE', #3826, 12.00000000001200462 ) ;
#8087 = VECTOR ( 'NONE', #13450, 1000.000000000000000 ) ;
#8088 = EDGE_CURVE ( 'NONE', #3360, #18126, #9438, .T. ) ;
#8089 = AXIS2_PLACEMENT_3D ( 'NONE', #8525, #1297, #6321 ) ;
#8090 = ORIENTED_EDGE ( 'NONE', *, *, #7130, .T. ) ;
#8091 = EDGE_CURVE ( 'NONE', #18552, #4170, #13640, .T. ) ;
#8092 = AXIS2_PLACEMENT_3D ( 'NONE', #2589, #8404, #16883 ) ;
#8093 = AXIS2_PLACEMENT_3D ( 'NONE', #16810, #3583, #16617 ) ;
#8094 = ORIENTED_EDGE ( 'NONE', *, *, #3172, .T. ) ;
#8095 = LINE ( 'NONE', #13910, #2337 ) ;
#8096 = CIRCLE ( 'NONE', #18746, 56.24900000005625600 ) ;
#8097 = FACE_OUTER_BOUND ( 'NONE', #10784, .T. ) ;
#8098 = VECTOR ( 'NONE', #16576, 999.9999999999998863 ) ;
#8099 = DIRECTION ( 'NONE',  ( 0.000000000000000000, 0.000000000000000000, 1.000000000000000000 ) ) ;
#8100 = CARTESIAN_POINT ( 'NONE',  ( 3.673940397442059178E-15, 0.000000000000000000, 30.00000000000000000 ) ) ;
#8101 = DIRECTION ( 'NONE',  ( 0.000000000000000000, -0.4999999999999992228, 0.8660254037844390407 ) ) ;
#8102 = CARTESIAN_POINT ( 'NONE',  ( -2.100000000000000089, 2.571758278209441957E-16, -4.694516984716113228 ) ) ;
#8103 = EDGE_LOOP ( 'NONE', ( #18176, #3418 ) ) ;
#8104 = DIRECTION ( 'NONE',  ( 0.000000000000000000, 0.000000000000000000, 1.000000000000000000 ) ) ;
#8105 = EDGE_CURVE ( 'NONE', #11121, #11814, #6397, .T. ) ;
#8106 = LINE ( 'NONE', #9728, #8472 ) ;
#8107 = ORIENTED_EDGE ( 'NONE', *, *, #16099, .F. ) ;
#8108 = AXIS2_PLACEMENT_3D ( 'NONE', #14804, #15095, #3102 ) ;
#8109 = ITEM_DEFINED_TRANSFORMATION ( 'NONE', 'NONE', #7755,  #8017 ) ;
#8110 = CIRCLE ( 'NONE', #7801, 56.24900000005625600 ) ;
#8111 = ORIENTED_EDGE ( 'NONE', *, *, #15403, .T. ) ;
#8112 = AXIS2_PLACEMENT_3D ( 'NONE', #6026, #321, #13178 ) ;
#8113 = AXIS2_PLACEMENT_3D ( 'NONE', #9898, #12771, #15719 ) ;
#8114 = ORIENTED_EDGE ( 'NONE', *, *, #3085, .F. ) ;
#8115 = ORIENTED_EDGE ( 'NONE', *, *, #5822, .F. ) ;
#8116 = FACE_OUTER_BOUND ( 'NONE', #2284, .T. ) ;
#8117 = DIRECTION ( 'NONE',  ( 0.000000000000000000, 0.1564344650402312575, -0.9876883405951376593 ) ) ;
#8118 = CARTESIAN_POINT ( 'NONE',  ( 0.000000000000000000, -33.95787273855213328, -45.00825343885058061 ) ) ;
#8119 = DIRECTION ( 'NONE',  ( -1.000000000000000000, -0.000000000000000000, -0.000000000000000000 ) ) ;
#8121 = DIRECTION ( 'NONE',  ( 0.000000000000000000, 0.000000000000000000, 1.000000000000000000 ) ) ;
#8120 = CIRCLE ( 'NONE', #9639, 2.649999999999985700 ) ;
#8122 = DIRECTION ( 'NONE',  ( -1.000000000000000000, -0.000000000000000000, -0.000000000000000000 ) ) ;
#8123 = CARTESIAN_POINT ( 'NONE',  ( 0.000000000000000000, -10.11537145609335653, -55.33199130079795225 ) ) ;
#8124 = VECTOR ( 'NONE', #5297, 1000.000000000000000 ) ;
#8125 = DIRECTION ( 'NONE',  ( 0.000000000000000000, 0.000000000000000000, 1.000000000000000000 ) ) ;
#8126 = EDGE_LOOP ( 'NONE', ( #11049, #1926 ) ) ;
#8127 = AXIS2_PLACEMENT_3D ( 'NONE', #12351, #15505, #654 ) ;
#8128 = DIRECTION ( 'NONE',  ( 0.000000000000000000, 0.000000000000000000, 1.000000000000000000 ) ) ;
#8129 = VERTEX_POINT ( 'NONE', #12487 ) ;
#8130 = EDGE_CURVE ( 'NONE', #10934, #451, #10857, .T. ) ;
#8131 = CARTESIAN_POINT ( 'NONE',  ( 10.00000000000000000, -34.13306034420217827, 44.70888270294149436 ) ) ;
#8132 = CYLINDRICAL_SURFACE ( 'NONE', #17871, 33.00000000003299760 ) ;
#8133 = ORIENTED_EDGE ( 'NONE', *, *, #17033, .T. ) ;
#8134 = ORIENTED_EDGE ( 'NONE', *, *, #7702, .T. ) ;
#8135 = DIRECTION ( 'NONE',  ( 0.000000000000000000, 0.000000000000000000, 1.000000000000000000 ) ) ;
#8136 = DIRECTION ( 'NONE',  ( -4.953800363085426557E-17, -1.000000000000000000, -3.599146639030026919E-17 ) ) ;
#8137 = CARTESIAN_POINT ( 'NONE',  ( -0.6937372685066653943, 4.453844082567723461, -3.610536846335889116 ) ) ;
#8138 = ORIENTED_EDGE ( 'NONE', *, *, #14359, .F. ) ;
#8139 = AXIS2_PLACEMENT_3D ( 'NONE', #4556, #3132, #14940 ) ;
#8140 = AXIS2_PLACEMENT_3D ( 'NONE', #18760, #7510, #15991 ) ;
#8141 = AXIS2_PLACEMENT_3D ( 'NONE', #12149, #4623, #10430 ) ;
#8142 = CIRCLE ( 'NONE', #11495, 2.649999999999995914 ) ;
#8143 = EDGE_CURVE ( 'NONE', #11877, #5078, #14503, .T. ) ;
#8144 = CARTESIAN_POINT ( 'NONE',  ( 10.00000000000000000, 20.41355805489643060, -19.44239304137353841 ) ) ;
#8145 = DIRECTION ( 'NONE',  ( 0.000000000000000000, 0.000000000000000000, 1.000000000000000000 ) ) ;
#8146 = DIRECTION ( 'NONE',  ( 0.000000000000000000, 0.000000000000000000, 1.000000000000000000 ) ) ;
#8147 = FACE_OUTER_BOUND ( 'NONE', #11800, .T. ) ;
#8148 = EDGE_CURVE ( 'NONE', #18105, #1178, #12390, .T. ) ;
#8149 = CIRCLE ( 'NONE', #14837, 26.24900000002624978 ) ;
#8150 = VERTEX_POINT ( 'NONE', #16780 ) ;
#8151 = CARTESIAN_POINT ( 'NONE',  ( 0.000000000000000000, -26.50000000000000000, 0.000000000000000000 ) ) ;
#8152 = EDGE_LOOP ( 'NONE', ( #12776, #512, #3798, #5876 ) ) ;
#8153 = AXIS2_PLACEMENT_3D ( 'NONE', #10977, #15561, #13836 ) ;
#8154 = CYLINDRICAL_SURFACE ( 'NONE', #4151, 24.00000000002399858 ) ;
#8155 = DIRECTION ( 'NONE',  ( 1.000000000000000000, 0.000000000000000000, 0.000000000000000000 ) ) ;
#8156 = DIRECTION ( 'NONE',  ( 1.000000000000000000, -0.000000000000000000, -0.000000000000000000 ) ) ;
#8157 = AXIS2_PLACEMENT_3D ( 'NONE', #6719, #5485, #12613 ) ;
#8158 = ORIENTED_EDGE ( 'NONE', *, *, #11514, .T. ) ;
#8159 = ORIENTED_EDGE ( 'NONE', *, *, #18080, .T. ) ;
#8160 = AXIS2_PLACEMENT_3D ( 'NONE', #6106, #7910, #677 ) ;
#8161 = DIRECTION ( 'NONE',  ( -1.000000000000000000, 0.000000000000000000, 0.000000000000000000 ) ) ;
#8162 = SHAPE_REPRESENTATION_RELATIONSHIP ( 'NONE' , 'NONE' ,  #2386, #10770 ) ;
#8163 = ORIENTED_EDGE ( 'NONE', *, *, #2202, .F. ) ;
#8164 = DIRECTION ( 'NONE',  ( 0.000000000000000000, 1.000000000000000000, -1.287488025362403787E-15 ) ) ;
#8165 = CIRCLE ( 'NONE', #15169, 4.349594641156948605 ) ;
#8166 = CIRCLE ( 'NONE', #9990, 12.00000000001200817 ) ;
#8167 = DIRECTION ( 'NONE',  ( 0.5000000000000013323, -0.8660254037844379305, 0.000000000000000000 ) ) ;
#8168 = AXIS2_PLACEMENT_3D ( 'NONE', #10202, #13162, #12790 ) ;
#8169 = CIRCLE ( 'NONE', #17905, 63.00000000006298961 ) ;
#8170 = CARTESIAN_POINT ( 'NONE',  ( 10.00000000000000000, -5.086963483077402870, 27.72801475327280585 ) ) ;
#8171 = ORIENTED_EDGE ( 'NONE', *, *, #6093, .F. ) ;
#8172 =( LENGTH_UNIT ( ) NAMED_UNIT ( * ) SI_UNIT ( .MILLI., .METRE. ) );
#8173 = VERTEX_POINT ( 'NONE', #5241 ) ;
#8174 = CARTESIAN_POINT ( 'NONE',  ( 10.04305231718605285, -34.99999999999999289, -30.90933677959240811 ) ) ;
#8175 = CARTESIAN_POINT ( 'NONE',  ( -0.2500000000000000000, -8.096141056083446585, -1.000000000000000000 ) ) ;
#8176 = CARTESIAN_POINT ( 'NONE',  ( 0.000000000000000000, -26.50000000000000000, 25.00000000000000000 ) ) ;
#8177 = ORIENTED_EDGE ( 'NONE', *, *, #3516, .F. ) ;
#8178 = CARTESIAN_POINT ( 'NONE',  ( 4.999999999999999112, -4.381479206523219538, 32.70783759231085241 ) ) ;
#8179 = ORIENTED_EDGE ( 'NONE', *, *, #5234, .T. ) ;
#8180 = CARTESIAN_POINT ( 'NONE',  ( 0.000000000000000000, -30.00000000000000000, 25.00000000000000000 ) ) ;
#8181 = DIRECTION ( 'NONE',  ( 0.000000000000000000, 0.000000000000000000, 1.000000000000000000 ) ) ;
#8182 = CIRCLE ( 'NONE', #6359, 2.649999999999995914 ) ;
#8183 = ORIENTED_EDGE ( 'NONE', *, *, #396, .F. ) ;
#8184 = ORIENTED_EDGE ( 'NONE', *, *, #18761, .F. ) ;
#8185 = CIRCLE ( 'NONE', #10002, 33.00000000003299760 ) ;
#8186 = VERTEX_POINT ( 'NONE', #11046 ) ;
#8187 = DIRECTION ( 'NONE',  ( -1.000000000000000000, -0.000000000000000000, -0.000000000000000000 ) ) ;
#8188 = LINE ( 'NONE', #13998, #4020 ) ;
#8189 = AXIS2_PLACEMENT_3D ( 'NONE', #2381, #3529, #9324 ) ;
#8190 = VECTOR ( 'NONE', #1523, 1000.000000000000000 ) ;
#8191 = EDGE_CURVE ( 'NONE', #10145, #15878, #8666, .T. ) ;
#8192 = EDGE_CURVE ( 'NONE', #15342, #9705, #18770, .T. ) ;
#8193 = EDGE_CURVE ( 'NONE', #17735, #5117, #15157, .T. ) ;
#8194 = EDGE_CURVE ( 'NONE', #2784, #14848, #17586, .T. ) ;
#8195 = ORIENTED_EDGE ( 'NONE', *, *, #3067, .F. ) ;
#8196 = AXIS2_PLACEMENT_3D ( 'NONE', #4727, #1513, #9013 ) ;
#8197 = ADVANCED_FACE ( 'NONE', ( #9821 ), #6960, .T. ) ;
#8198 = ORIENTED_EDGE ( 'NONE', *, *, #15995, .T. ) ;
#8199 = DIRECTION ( 'NONE',  ( 0.000000000000000000, 0.1564344650402243464, 0.9876883405951388806 ) ) ;
#8200 = CARTESIAN_POINT ( 'NONE',  ( -0.3865131578947368918, -23.49682122285426189, -2.000000000000000000 ) ) ;
#8201 = DIRECTION ( 'NONE',  ( -1.000000000000000000, -0.000000000000000000, -0.000000000000000000 ) ) ;
#8202 = FACE_BOUND ( 'NONE', #17901, .T. ) ;
#8203 = ADVANCED_FACE ( 'NONE', ( #12678, #12965 ), #2776, .T. ) ;
#8204 = CARTESIAN_POINT ( 'NONE',  ( -79.64793068852927149, -34.99999999999999289, 29.21039329588765554 ) ) ;
#8205 = DIRECTION ( 'NONE',  ( 0.000000000000000000, 0.000000000000000000, 1.000000000000000000 ) ) ;
#8206 = CYLINDRICAL_SURFACE ( 'NONE', #14182, 2.649999999999999467 ) ;
#8207 = EDGE_LOOP ( 'NONE', ( #4576, #8409, #1048, #18510 ) ) ;
#8208 = DIRECTION ( 'NONE',  ( -1.000000000000000000, 0.000000000000000000, 0.000000000000000000 ) ) ;
#8209 = DIRECTION ( 'NONE',  ( 0.000000000000000000, 0.000000000000000000, 1.000000000000000000 ) ) ;
#8210 = DIRECTION ( 'NONE',  ( 0.000000000000000000, 0.000000000000000000, 1.000000000000000000 ) ) ;
#8211 = CARTESIAN_POINT ( 'NONE',  ( 10.00000000000000000, -44.70888270294186384, 34.13306034420170931 ) ) ;
#8212 = EDGE_CURVE ( 'NONE', #5044, #18322, #4301, .T. ) ;
#8213 = ITEM_DEFINED_TRANSFORMATION ( 'NONE', 'NONE', #6842,  #8017 ) ;
#8214 = AXIS2_PLACEMENT_3D ( 'NONE', #697, #2029, #11056 ) ;
#8215 = EDGE_CURVE ( 'NONE', #205, #6839, #1786, .T. ) ;
#8216 = ORIENTED_EDGE ( 'NONE', *, *, #1296, .T. ) ;
#8217 = VERTEX_POINT ( 'NONE', #7240 ) ;
#8218 = ADVANCED_FACE ( 'NONE', ( #13062 ), #10012, .T. ) ;
#8219 = ORIENTED_EDGE ( 'NONE', *, *, #44, .F. ) ;
#8220 = CARTESIAN_POINT ( 'NONE',  ( 10.00000000000000000, -24.33982105418938602, 50.71018745830434682 ) ) ;
#8221 = DIRECTION ( 'NONE',  ( 0.000000000000000000, 0.000000000000000000, 1.000000000000000000 ) ) ;
#8222 = CIRCLE ( 'NONE', #9421, 24.00000000002399858 ) ;
#8223 = CARTESIAN_POINT ( 'NONE',  ( 12.49999999999999289, 0.000000000000000000, 0.000000000000000000 ) ) ;
#8224 = FACE_OUTER_BOUND ( 'NONE', #8782, .T. ) ;
#8225 = VECTOR ( 'NONE', #11282, 1000.000000000000000 ) ;
#8226 = SURFACE_SIDE_STYLE ('',( #7926 ) ) ;
#8227 = DIRECTION ( 'NONE',  ( -1.000000000000000000, -0.000000000000000000, -0.000000000000000000 ) ) ;
#8228 = CARTESIAN_POINT ( 'NONE',  ( -79.64793068852898728, -30.00000000000000000, -34.51039329588755322 ) ) ;
#8229 = DIRECTION ( 'NONE',  ( -1.000000000000000000, 0.000000000000000000, 0.000000000000000000 ) ) ;
#8230 = ORIENTED_EDGE ( 'NONE', *, *, #10736, .F. ) ;
#8231 = CARTESIAN_POINT ( 'NONE',  ( 0.000000000000000000, 0.000000000000000000, 0.000000000000000000 ) ) ;
#8232 = ORIENTED_EDGE ( 'NONE', *, *, #14283, .F. ) ;
#8233 = FACE_OUTER_BOUND ( 'NONE', #13260, .T. ) ;
#8234 = DIRECTION ( 'NONE',  ( -0.000000000000000000, 1.000000000000000000, -0.000000000000000000 ) ) ;
#8235 = ORIENTED_EDGE ( 'NONE', *, *, #372, .F. ) ;
#8236 = ORIENTED_EDGE ( 'NONE', *, *, #16562, .F. ) ;
#8237 = DIRECTION ( 'NONE',  ( 0.000000000000000000, 1.224646799147353207E-16, 1.000000000000000000 ) ) ;
#8238 = CARTESIAN_POINT ( 'NONE',  ( 45.00000000000000000, 15.00000000000001599, -5.120903701083534543E-13 ) ) ;
#8239 = CARTESIAN_POINT ( 'NONE',  ( 0.5000000000000000000, -6.429618962271402616, -1.000000000000000000 ) ) ;
#8240 = ORIENTED_EDGE ( 'NONE', *, *, #1019, .F. ) ;
#8241 = AXIS2_PLACEMENT_3D ( 'NONE', #12210, #6592, #18018 ) ;
#8242 = EDGE_CURVE ( 'NONE', #1465, #1879, #14264, .T. ) ;
#8243 = CYLINDRICAL_SURFACE ( 'NONE', #8093, 63.00000000006298961 ) ;
#8244 = DIRECTION ( 'NONE',  ( 0.000000000000000000, 0.000000000000000000, 1.000000000000000000 ) ) ;
#8245 = DIRECTION ( 'NONE',  ( 0.000000000000000000, 0.000000000000000000, -1.000000000000000000 ) ) ;
#8246 = DIRECTION ( 'NONE',  ( 0.000000000000000000, 0.000000000000000000, 1.000000000000000000 ) ) ;
#8247 = ORIENTED_EDGE ( 'NONE', *, *, #1001, .T. ) ;
#8248 = DIRECTION ( 'NONE',  ( -0.000000000000000000, 1.000000000000000000, -0.000000000000000000 ) ) ;
#8249 = EDGE_LOOP ( 'NONE', ( #17849, #10842, #5611, #2417, #17451 ) ) ;
#8250 = VECTOR ( 'NONE', #1715, 1000.000000000000000 ) ;
#8251 = CARTESIAN_POINT ( 'NONE',  ( -10.00000000000000000, 0.000000000000000000, 0.000000000000000000 ) ) ;
#8252 = CARTESIAN_POINT ( 'NONE',  ( 10.00000000000000000, 22.07705612348840063, 14.19907017806876404 ) ) ;
#8253 = CARTESIAN_POINT ( 'NONE',  ( 11.25000000000000000, 0.000000000000000000, -28.00000000000000355 ) ) ;
#8254 = ORIENTED_EDGE ( 'NONE', *, *, #8875, .T. ) ;
#8255 = EDGE_LOOP ( 'NONE', ( #640, #6833 ) ) ;
#8256 = SHAPE_REPRESENTATION ( 'socket head cap screw_iso_ISO 4762 M5 x 16 - 16N', ( #8017 ), #7430 ) ;
#8257 = LINE ( 'NONE', #9488, #5944 ) ;
#8258 = FILL_AREA_STYLE_COLOUR ( '', #14143 ) ;
#8259 = EDGE_CURVE ( 'NONE', #1496, #8307, #18674, .T. ) ;
#8260 = ORIENTED_EDGE ( 'NONE', *, *, #14834, .F. ) ;
#8261 = LINE ( 'NONE', #1118, #11561 ) ;
#8262 = EDGE_CURVE ( 'NONE', #15093, #3414, #6861, .T. ) ;
#8263 = AXIS2_PLACEMENT_3D ( 'NONE', #10901, #16729, #8246 ) ;
#8264 = CYLINDRICAL_SURFACE ( 'NONE', #18413, 25.00000000000000000 ) ;
#8265 = CARTESIAN_POINT ( 'NONE',  ( -4.799999999999999822, 5.878304635907294211E-16, -1.000000000000000000 ) ) ;
#8266 = ORIENTED_EDGE ( 'NONE', *, *, #15061, .T. ) ;
#8267 = CARTESIAN_POINT ( 'NONE',  ( 10.00000000000000000, -19.44239304137390434, 20.41355805489607889 ) ) ;
#8268 = CIRCLE ( 'NONE', #12835, 23.50000000000001066 ) ;
#8269 = ORIENTED_EDGE ( 'NONE', *, *, #17483, .T. ) ;
#8270 = CARTESIAN_POINT ( 'NONE',  ( 0.6810597143197052450, 4.461075778259290914, -3.598441714920602053 ) ) ;
#8271 = DIRECTION ( 'NONE',  ( 0.000000000000000000, 0.000000000000000000, 1.000000000000000000 ) ) ;
#8272 = CARTESIAN_POINT ( 'NONE',  ( 0.000000000000000000, 0.000000000000000000, 0.000000000000000000 ) ) ;
#8273 = ORIENTED_EDGE ( 'NONE', *, *, #18511, .T. ) ;
#8274 = CARTESIAN_POINT ( 'NONE',  ( 0.000000000000000000, -15.61693798565454827, -61.03368945066451801 ) ) ;
#8275 = VERTEX_POINT ( 'NONE', #14202 ) ;
#8276 = CARTESIAN_POINT ( 'NONE',  ( 5.000000000000000000, -32.70783759231083820, -4.381479206523334113 ) ) ;
#8277 = DIRECTION ( 'NONE',  ( 0.000000000000000000, 0.000000000000000000, 1.000000000000000000 ) ) ;
#8278 = ORIENTED_EDGE ( 'NONE', *, *, #2375, .T. ) ;
#8279 = ORIENTED_EDGE ( 'NONE', *, *, #7362, .T. ) ;
#8280 = DIRECTION ( 'NONE',  ( 0.000000000000000000, 0.7071067811865439090, 0.7071067811865511255 ) ) ;
#8281 = ORIENTED_EDGE ( 'NONE', *, *, #3241, .F. ) ;
#8282 = DIRECTION ( 'NONE',  ( -1.000000000000000000, -0.000000000000000000, -0.000000000000000000 ) ) ;
#8283 = DIRECTION ( 'NONE',  ( 0.000000000000000000, 0.000000000000000000, 1.000000000000000000 ) ) ;
#8284 = APPLICATION_CONTEXT ( 'automotive_design' ) ;
#8285 = EDGE_LOOP ( 'NONE', ( #2116, #15378, #1335, #9368 ) ) ;
#8286 = EDGE_LOOP ( 'NONE', ( #10468, #3915, #18260, #4539 ) ) ;
#8287 = DIRECTION ( 'NONE',  ( 0.000000000000000000, 0.000000000000000000, 1.000000000000000000 ) ) ;
#8288 = CARTESIAN_POINT ( 'NONE',  ( 4.000000000000000000, -2.511475576507276042, -3.469253905236643565 ) ) ;
#8289 = LINE ( 'NONE', #18284, #2328 ) ;
#8290 = FACE_OUTER_BOUND ( 'NONE', #8979, .T. ) ;
#8291 = ADVANCED_FACE ( 'NONE', ( #5451 ), #11434, .F. ) ;
#8292 = AXIS2_PLACEMENT_3D ( 'NONE', #15139, #16469, #6375 ) ;
#8293 = EDGE_CURVE ( 'NONE', #5770, #9182, #17255, .T. ) ;
#8294 = CARTESIAN_POINT ( 'NONE',  ( -3.309651814758565180, -5.455921364805393026, -1.000000000000000000 ) ) ;
#8295 = CARTESIAN_POINT ( 'NONE',  ( 5.000000000000000000, 29.75305054077492173, -14.27431201565494767 ) ) ;
#8296 = CARTESIAN_POINT ( 'NONE',  ( 4.000000000000003553, -2.309401076758513138, -3.504271511727127031 ) ) ;
#8297 = ORIENTED_EDGE ( 'NONE', *, *, #13017, .T. ) ;
#8298 = CARTESIAN_POINT ( 'NONE',  ( -0.1481481481481481122, -4.797713218419819903, 0.000000000000000000 ) ) ;
#8299 = DIRECTION ( 'NONE',  ( 0.04803802292983955224, 0.000000000000000000, -0.9988455077503187729 ) ) ;
#8300 = PRODUCT_DEFINITION ( 'UNKNOWN', '', #10485, #1225 ) ;
#8301 = CARTESIAN_POINT ( 'NONE',  ( 10.00000000000000000, -45.00825343885045271, 33.95787273855228960 ) ) ;
#8302 = CARTESIAN_POINT ( 'NONE',  ( 10.00000000000000000, -27.72801475327278453, 6.913036516934497833 ) ) ;
#8303 = ADVANCED_BREP_SHAPE_REPRESENTATION ( '', ( #9854, #8017 ), #2559 ) ;
#8304 = EDGE_CURVE ( 'NONE', #276, #2784, #2573, .T. ) ;
#8305 = EDGE_LOOP ( 'NONE', ( #17888, #1347, #7185, #14407 ) ) ;
#8306 = AXIS2_PLACEMENT_3D ( 'NONE', #16074, #3030, #15886 ) ;
#8307 = VERTEX_POINT ( 'NONE', #4210 ) ;
#8308 = EDGE_CURVE ( 'NONE', #168, #8012, #5755, .T. ) ;
#8309 = AXIS2_PLACEMENT_3D ( 'NONE', #15645, #14220, #3743 ) ;
#8310 = AXIS2_PLACEMENT_3D ( 'NONE', #7989, #2182, #763 ) ;
#8311 = ORIENTED_EDGE ( 'NONE', *, *, #14187, .F. ) ;
#8312 = DIRECTION ( 'NONE',  ( 0.000000000000000000, -0.5000000000000013323, -0.8660254037844380415 ) ) ;
#8313 = SURFACE_STYLE_USAGE ( .BOTH. , #2584 ) ;
#8314 = DIRECTION ( 'NONE',  ( 0.000000000000000000, 0.000000000000000000, -1.000000000000000000 ) ) ;
#8315 = ADVANCED_FACE ( 'NONE', ( #8393 ), #15826, .F. ) ;
#8316 = DIRECTION ( 'NONE',  ( 1.000000000000000000, 0.000000000000000000, 0.000000000000000000 ) ) ;
#8317 = ADVANCED_FACE ( 'NONE', ( #7699 ), #11985, .T. ) ;
#8318 = FACE_OUTER_BOUND ( 'NONE', #11196, .T. ) ;
#8319 = CARTESIAN_POINT ( 'NONE',  ( 10.00000000000000000, -61.47135697633788709, 13.79392154159114092 ) ) ;
#8320 = DIRECTION ( 'NONE',  ( 0.000000000000000000, 0.000000000000000000, 1.000000000000000000 ) ) ;
#8321 = ORIENTED_EDGE ( 'NONE', *, *, #13363, .F. ) ;
#8322 = DIRECTION ( 'NONE',  ( 1.000000000000000000, 0.000000000000000000, 0.000000000000000000 ) ) ;
#8323 = ORIENTED_EDGE ( 'NONE', *, *, #10175, .F. ) ;
#8324 = AXIS2_PLACEMENT_3D ( 'NONE', #1571, #1381, #3008 ) ;
#8325 = ADVANCED_FACE ( 'NONE', ( #16103, #16279 ), #3238, .T. ) ;
#8326 = CARTESIAN_POINT ( 'NONE',  ( 0.000000000000000000, -38.81885513160016643, 40.70683587897944022 ) ) ;
#8327 = CARTESIAN_POINT ( 'NONE',  ( -12.69999999999999929, 0.000000000000000000, -27.00000000000000355 ) ) ;
#8328 = VERTEX_POINT ( 'NONE', #196 ) ;
#8329 = ADVANCED_FACE ( 'NONE', ( #4754 ), #4662, .F. ) ;
#8330 = CARTESIAN_POINT ( 'NONE',  ( 10.00000000000000000, -53.29895248911662264, -18.38754094778296277 ) ) ;
#8331 = CARTESIAN_POINT ( 'NONE',  ( 10.04305231718534763, -39.99999999999999289, 30.90933677959263193 ) ) ;
#8332 = CARTESIAN_POINT ( 'NONE',  ( 5.686050877451574337, -5.768780236673276995, -1.000000000000000000 ) ) ;
#8333 = ORIENTED_EDGE ( 'NONE', *, *, #7021, .F. ) ;
#8334 = EDGE_CURVE ( 'NONE', #17956, #13691, #1706, .T. ) ;
#8335 = CIRCLE ( 'NONE', #1634, 56.24900000005625600 ) ;
#8336 = DIRECTION ( 'NONE',  ( -0.000000000000000000, 1.000000000000000000, -0.000000000000000000 ) ) ;
#8337 = DIRECTION ( 'NONE',  ( -0.000000000000000000, 1.000000000000000000, -0.000000000000000000 ) ) ;
#8338 = LINE ( 'NONE', #5279, #9338 ) ;
#8339 = CARTESIAN_POINT ( 'NONE',  ( 10.00000000000000000, 0.000000000000000000, 0.000000000000000000 ) ) ;
#8340 = FACE_OUTER_BOUND ( 'NONE', #7638, .T. ) ;
#8341 = ORIENTED_EDGE ( 'NONE', *, *, #14602, .T. ) ;
#8342 = CARTESIAN_POINT ( 'NONE',  ( 10.00000000000000000, 7.813799127874054840, -55.83748330407399152 ) ) ;
#8343 = DIRECTION ( 'NONE',  ( 0.000000000000000000, 0.000000000000000000, 1.000000000000000000 ) ) ;
#8344 = CARTESIAN_POINT ( 'NONE',  ( 0.000000000000000000, 49.76630880786309064, 26.49895292618021614 ) ) ;
#8345 = ORIENTED_EDGE ( 'NONE', *, *, #11334, .T. ) ;
#8346 = ORIENTED_EDGE ( 'NONE', *, *, #18566, .F. ) ;
#8347 = EDGE_CURVE ( 'NONE', #10140, #3048, #11205, .T. ) ;
#8348 = DIRECTION ( 'NONE',  ( 0.000000000000000000, -1.000000000000000000, -1.040834085585043434E-14 ) ) ;
#8349 = ORIENTED_EDGE ( 'NONE', *, *, #8644, .T. ) ;
#8350 = DIRECTION ( 'NONE',  ( -1.000000000000000000, -0.000000000000000000, -0.000000000000000000 ) ) ;
#8351 = CARTESIAN_POINT ( 'NONE',  ( 0.000000000000000000, -3.730438010304114371, -27.94286728106396822 ) ) ;
#8352 = CARTESIAN_POINT ( 'NONE',  ( 32.50000000000000000, -30.00000000000000000, 2.650000000000367617 ) ) ;
#8353 = EDGE_LOOP ( 'NONE', ( #16636, #1593, #9713, #13305 ) ) ;
#8354 = CARTESIAN_POINT ( 'NONE',  ( 32.50000000000000000, -34.99999999999999289, -2.649999999999631317 ) ) ;
#8355 = EDGE_LOOP ( 'NONE', ( #16837, #3053 ) ) ;
#8356 = CARTESIAN_POINT ( 'NONE',  ( 5.000000000000000000, 62.87238730325621106, -4.007856633823612569 ) ) ;
#8357 = CARTESIAN_POINT ( 'NONE',  ( -36.40576474687247099, 0.000000000000000000, 29.10033635316149514 ) ) ;
#8358 = DIRECTION ( 'NONE',  ( -1.000000000000000000, 0.000000000000000000, 0.000000000000000000 ) ) ;
#8359 = AXIS2_PLACEMENT_3D ( 'NONE', #17513, #5893, #3224 ) ;
#8360 = ORIENTED_EDGE ( 'NONE', *, *, #6683, .T. ) ;
#8361 = DIRECTION ( 'NONE',  ( 0.9988455077503188839, 0.000000000000000000, 0.04803802292983956612 ) ) ;
#8362 = VERTEX_POINT ( 'NONE', #14860 ) ;
#8363 = CARTESIAN_POINT ( 'NONE',  ( -1.250000000000000000, -6.429618962271402616, -1.000000000000000000 ) ) ;
#8364 = DIRECTION ( 'NONE',  ( 0.000000000000000000, 0.000000000000000000, -1.000000000000000000 ) ) ;
#8365 = EDGE_LOOP ( 'NONE', ( #11090, #15634, #6145, #16264, #1631 ) ) ;
#8366 = ORIENTED_EDGE ( 'NONE', *, *, #6267, .F. ) ;
#8367 = EDGE_CURVE ( 'NONE', #5418, #16626, #13349, .T. ) ;
#8368 = CYLINDRICAL_SURFACE ( 'NONE', #4459, 12.00000000001200462 ) ;
#8369 = EDGE_LOOP ( 'NONE', ( #9359, #17848, #13383, #5035 ) ) ;
#8370 = CARTESIAN_POINT ( 'NONE',  ( -10.00000000000000000, -42.79754323328189969, -16.55576474687263300 ) ) ;
#8371 = CYLINDRICAL_SURFACE ( 'NONE', #7958, 56.24900000005625600 ) ;
#8372 = MECHANICAL_DESIGN_GEOMETRIC_PRESENTATION_REPRESENTATION (  '', ( #18083 ), #16573 ) ;
#8373 = CIRCLE ( 'NONE', #5006, 27.00000000000000000 ) ;
#8374 = VECTOR ( 'NONE', #8633, 1000.000000000000000 ) ;
#8375 = EDGE_CURVE ( 'NONE', #5515, #14782, #3006, .T. ) ;
#8376 = EDGE_LOOP ( 'NONE', ( #13659, #2480, #12817, #15187, #14989, #7146, #16522, #12142, #16899, #17695, #1189, #5812, #2636, #8052, #14411, #5022 ) ) ;
#8377 = AXIS2_PLACEMENT_3D ( 'NONE', #12059, #13692, #12248 ) ;
#8378 = ORIENTED_EDGE ( 'NONE', *, *, #12573, .T. ) ;
#8379 = DIRECTION ( 'NONE',  ( -1.000000000000000000, 0.000000000000000000, -0.000000000000000000 ) ) ;
#8380 = CARTESIAN_POINT ( 'NONE',  ( 0.000000000000000000, 23.88582760061514776, -22.76987570971501640 ) ) ;
#8381 = FACE_OUTER_BOUND ( 'NONE', #12103, .T. ) ;
#8382 = DIRECTION ( 'NONE',  ( 0.000000000000000000, 0.000000000000000000, 1.000000000000000000 ) ) ;
#8383 = EDGE_CURVE ( 'NONE', #2692, #2531, #16386, .T. ) ;
#8384 = VECTOR ( 'NONE', #4199, 1000.000000000000000 ) ;
#8385 = LINE ( 'NONE', #9618, #17884 ) ;
#8386 = DIRECTION ( 'NONE',  ( -1.000000000000000000, 0.000000000000000000, 0.000000000000000000 ) ) ;
#8387 = CIRCLE ( 'NONE', #12329, 5.000000000000000000 ) ;
#8388 = DIRECTION ( 'NONE',  ( -1.000000000000000000, 0.000000000000000000, 0.000000000000000000 ) ) ;
#8389 = VERTEX_POINT ( 'NONE', #3344 ) ;
#8390 = FACE_OUTER_BOUND ( 'NONE', #16147, .T. ) ;
#8391 = VECTOR ( 'NONE', #12985, 1000.000000000000000 ) ;
#8392 = LINE ( 'NONE', #9263, #1992 ) ;
#8393 = FACE_OUTER_BOUND ( 'NONE', #10007, .T. ) ;
#8394 = CARTESIAN_POINT ( 'NONE',  ( 2.354826896168714434, -6.962563485461402024, 0.000000000000000000 ) ) ;
#8395 = ORIENTED_EDGE ( 'NONE', *, *, #7658, .T. ) ;
#8396 = AXIS2_PLACEMENT_3D ( 'NONE', #3014, #2816, #8622 ) ;
#8397 = EDGE_LOOP ( 'NONE', ( #1884, #11855, #1312, #662 ) ) ;
#8398 = CIRCLE ( 'NONE', #5666, 24.00000000002399858 ) ;
#8399 = AXIS2_PLACEMENT_3D ( 'NONE', #10457, #8934, #191 ) ;
#8400 = ORIENTED_EDGE ( 'NONE', *, *, #16766, .T. ) ;
#8401 = DIRECTION ( 'NONE',  ( 0.000000000000000000, 0.000000000000000000, 1.000000000000000000 ) ) ;
#8402 = EDGE_LOOP ( 'NONE', ( #6830, #17340, #16217, #11165 ) ) ;
#8403 = DIRECTION ( 'NONE',  ( 0.000000000000000000, 0.000000000000000000, 1.000000000000000000 ) ) ;
#8404 = DIRECTION ( 'NONE',  ( -0.000000000000000000, -0.000000000000000000, -1.000000000000000000 ) ) ;
#8405 = LINE ( 'NONE', #4584, #13627 ) ;
#8406 = CARTESIAN_POINT ( 'NONE',  ( 0.000000000000000000, 0.000000000000000000, 0.000000000000000000 ) ) ;
#8407 = VECTOR ( 'NONE', #10424, 1000.000000000000000 ) ;
#8408 = CARTESIAN_POINT ( 'NONE',  ( 0.000000000000000000, 0.000000000000000000, 0.000000000000000000 ) ) ;
#8409 = ORIENTED_EDGE ( 'NONE', *, *, #7723, .F. ) ;
#8410 = CARTESIAN_POINT ( 'NONE',  ( -2.250000000000000000, -27.60846790388774608, -2.000000000000000000 ) ) ;
#8411 = VERTEX_POINT ( 'NONE', #9139 ) ;
#8412 = CIRCLE ( 'NONE', #11752, 7.500000000000007105 ) ;
#8413 = LINE ( 'NONE', #4132, #13507 ) ;
#8414 = DIRECTION ( 'NONE',  ( -1.000000000000000000, 0.000000000000000000, 0.000000000000000000 ) ) ;
#8415 = ORIENTED_EDGE ( 'NONE', *, *, #6140, .T. ) ;
#8416 = AXIS2_PLACEMENT_3D ( 'NONE', #6591, #12402, #18214 ) ;
#8417 = AXIS2_PLACEMENT_3D ( 'NONE', #3867, #17022, #6631 ) ;
#8418 = CARTESIAN_POINT ( 'NONE',  ( 34.99999999999999289, 0.000000000000000000, 0.000000000000000000 ) ) ;
#8419 = CARTESIAN_POINT ( 'NONE',  ( -36.40576474687270547, -14.99999999999999289, -26.45033635316118747 ) ) ;
#8420 = CARTESIAN_POINT ( 'NONE',  ( 23.50000000000000355, 0.000000000000000000, -2.000000000000000000 ) ) ;
#8421 = ORIENTED_EDGE ( 'NONE', *, *, #2354, .T. ) ;
#8422 = EDGE_CURVE ( 'NONE', #5360, #596, #265, .T. ) ;
#8423 = EDGE_CURVE ( 'NONE', #16326, #13451, #11533, .T. ) ;
#8424 = EDGE_CURVE ( 'NONE', #9696, #9657, #892, .T. ) ;
#8425 = AXIS2_PLACEMENT_3D ( 'NONE', #16859, #2380, #8199 ) ;
#8426 = AXIS2_PLACEMENT_3D ( 'NONE', #16759, #12654, #3710 ) ;
#8427 = VECTOR ( 'NONE', #15156, 1000.000000000000000 ) ;
#8428 = DIRECTION ( 'NONE',  ( 0.000000000000000000, -0.3090169943749348502, -0.9510565162951576390 ) ) ;
#8429 = EDGE_CURVE ( 'NONE', #16875, #186, #3920, .T. ) ;
#8430 = CARTESIAN_POINT ( 'NONE',  ( -117.1020693116508085, -34.99999999999999289, 19.69080595179778115 ) ) ;
#8431 = VECTOR ( 'NONE', #2103, 1000.000000000000000 ) ;
#8432 = DIRECTION ( 'NONE',  ( 0.000000000000000000, 0.000000000000000000, -1.000000000000000000 ) ) ;
#8433 = DIRECTION ( 'NONE',  ( -1.000000000000000000, 0.000000000000000000, -0.000000000000000000 ) ) ;
#8434 = EDGE_CURVE ( 'NONE', #15653, #3994, #15784, .T. ) ;
#8435 = DIRECTION ( 'NONE',  ( 1.000000000000000000, 0.000000000000000000, 0.000000000000000000 ) ) ;
#8436 = ORIENTED_EDGE ( 'NONE', *, *, #917, .T. ) ;
#8437 = DIRECTION ( 'NONE',  ( -2.031314180040284764E-16, -1.000000000000000000, -1.301042606982601377E-16 ) ) ;
#8438 = DIRECTION ( 'NONE',  ( 0.000000000000000000, 0.000000000000000000, 1.000000000000000000 ) ) ;
#8439 = DIRECTION ( 'NONE',  ( 1.000000000000000000, 0.000000000000000000, 0.000000000000000000 ) ) ;
#8440 = AXIS2_PLACEMENT_3D ( 'NONE', #9211, #7604, #11974 ) ;
#8441 = VERTEX_POINT ( 'NONE', #16192 ) ;
#8442 = EDGE_LOOP ( 'NONE', ( #10159, #17865, #10011, #9570 ) ) ;
#8443 = CYLINDRICAL_SURFACE ( 'NONE', #12342, 24.00000000002399503 ) ;
#8444 = SURFACE_SIDE_STYLE ('',( #6818 ) ) ;
#8445 = AXIS2_PLACEMENT_3D ( 'NONE', #6513, #13950, #18321 ) ;
#8446 = ORIENTED_EDGE ( 'NONE', *, *, #6782, .T. ) ;
#8447 = CYLINDRICAL_SURFACE ( 'NONE', #15812, 24.00000000002399858 ) ;
#8448 = EDGE_CURVE ( 'NONE', #3135, #16274, #8185, .T. ) ;
#8449 = CARTESIAN_POINT ( 'NONE',  ( 6.735557395310442615E-15, 3.000000000000000000, 55.00000000000000000 ) ) ;
#8450 = CIRCLE ( 'NONE', #10866, 1.249999999999999778 ) ;
#8451 = DIRECTION ( 'NONE',  ( 0.000000000000000000, 0.000000000000000000, 1.000000000000000000 ) ) ;
#8452 = EDGE_CURVE ( 'NONE', #726, #7504, #11717, .T. ) ;
#8453 = ORIENTED_EDGE ( 'NONE', *, *, #15278, .T. ) ;
#8454 = DIRECTION ( 'NONE',  ( 0.000000000000000000, 0.000000000000000000, 1.000000000000000000 ) ) ;
#8455 = CIRCLE ( 'NONE', #14838, 23.50000000000001066 ) ;
#8456 = ORIENTED_EDGE ( 'NONE', *, *, #11861, .T. ) ;
#8457 = DIRECTION ( 'NONE',  ( 0.9396926207859138680, 1.150791560227856926E-16, -0.3420201433256536139 ) ) ;
#8458 = CARTESIAN_POINT ( 'NONE',  ( 0.000000000000000000, 0.000000000000000000, 0.000000000000000000 ) ) ;
#8459 = CARTESIAN_POINT ( 'NONE',  ( -117.1020693116506379, -34.99999999999999289, -22.34080595179800355 ) ) ;
#8460 = ORIENTED_EDGE ( 'NONE', *, *, #1001, .F. ) ;
#8461 = FACE_BOUND ( 'NONE', #11970, .T. ) ;
#8462 = ORIENTED_EDGE ( 'NONE', *, *, #1559, .F. ) ;
#8463 = CARTESIAN_POINT ( 'NONE',  ( -0.1481481481481481122, -4.797713218419819903, -1.000000000000000000 ) ) ;
#8464 = DIRECTION ( 'NONE',  ( 0.000000000000000000, 0.1564344650402244297, 0.9876883405951387696 ) ) ;
#8465 = VERTEX_POINT ( 'NONE', #7420 ) ;
#8466 = EDGE_LOOP ( 'NONE', ( #9781, #12506 ) ) ;
#8467 = DIRECTION ( 'NONE',  ( -1.000000000000000000, 0.000000000000000000, 0.000000000000000000 ) ) ;
#8468 = ORIENTED_EDGE ( 'NONE', *, *, #13180, .F. ) ;
#8469 = CARTESIAN_POINT ( 'NONE',  ( 0.000000000000000000, 26.45033635316149301, 36.40576474687247099 ) ) ;
#8470 = DIRECTION ( 'NONE',  ( -1.000000000000000000, -0.000000000000000000, -0.000000000000000000 ) ) ;
#8471 = CIRCLE ( 'NONE', #12110, 33.00000000003299760 ) ;
#8472 = VECTOR ( 'NONE', #15539, 1000.000000000000000 ) ;
#8473 = CIRCLE ( 'NONE', #252, 27.29487558977753991 ) ;
#8474 = EDGE_CURVE ( 'NONE', #1940, #11202, #4570, .T. ) ;
#8475 = EDGE_LOOP ( 'NONE', ( #4994, #13413, #2276, #8732 ) ) ;
#8476 = ORIENTED_EDGE ( 'NONE', *, *, #15774, .F. ) ;
#8477 = DIRECTION ( 'NONE',  ( 0.000000000000000000, 0.000000000000000000, 1.000000000000000000 ) ) ;
#8478 = CARTESIAN_POINT ( 'NONE',  ( -0.6920835326022555245, -4.454600218803899558, -3.597382984111586079 ) ) ;
#8479 = CARTESIAN_POINT ( 'NONE',  ( 2.500000000000000000, 1.178949249685213863, -2.042000000000001148 ) ) ;
#8480 = FACE_OUTER_BOUND ( 'NONE', #7397, .T. ) ;
#8481 = AXIS2_PLACEMENT_3D ( 'NONE', #12560, #13800, #6665 ) ;
#8482 = CARTESIAN_POINT ( 'NONE',  ( 0.000000000000000000, -62.72529079327811274, 5.876895005582225551 ) ) ;
#8483 = CARTESIAN_POINT ( 'NONE',  ( 4.000000000000000000, -2.309401076758514915, -5.000000000000000000 ) ) ;
#8484 = AXIS2_PLACEMENT_3D ( 'NONE', #12854, #5607, #7656 ) ;
#8485 = CARTESIAN_POINT ( 'NONE',  ( 4.101954839143203912, -2.368264730583031330, -3.681130640444377988 ) ) ;
#8486 = ORIENTED_EDGE ( 'NONE', *, *, #5992, .F. ) ;
#8487 = AXIS2_PLACEMENT_3D ( 'NONE', #14567, #11535, #17153 ) ;
#8488 = CARTESIAN_POINT ( 'NONE',  ( 0.000000000000000000, 11.24999999999999645, 25.00000000000000000 ) ) ;
#8489 = CARTESIAN_POINT ( 'NONE',  ( 10.00000000000000000, 4.007856633824264492, -62.87238730325616132 ) ) ;
#8490 = DIRECTION ( 'NONE',  ( -1.000000000000000000, 0.000000000000000000, 0.000000000000000000 ) ) ;
#8491 = DIRECTION ( 'NONE',  ( -1.000000000000000000, 0.000000000000000000, 0.000000000000000000 ) ) ;
#8492 = EDGE_CURVE ( 'NONE', #11257, #3135, #13645, .T. ) ;
#8493 = ORIENTED_EDGE ( 'NONE', *, *, #4388, .F. ) ;
#8494 = AXIS2_PLACEMENT_3D ( 'NONE', #8410, #11644, #2505 ) ;
#8495 = CIRCLE ( 'NONE', #13367, 4.250000000000000000 ) ;
#8496 = EDGE_CURVE ( 'NONE', #12688, #11921, #13053, .T. ) ;
#8497 = ORIENTED_EDGE ( 'NONE', *, *, #15242, .F. ) ;
#8498 = CYLINDRICAL_SURFACE ( 'NONE', #9310, 12.00000000001200817 ) ;
#8499 = LINE ( 'NONE', #18389, #9436 ) ;
#8500 = VERTEX_POINT ( 'NONE', #3625 ) ;
#8501 = DIRECTION ( 'NONE',  ( 0.000000000000000000, 0.000000000000000000, 1.000000000000000000 ) ) ;
#8502 = CARTESIAN_POINT ( 'NONE',  ( 0.000000000000000000, -44.70888270294185673, 34.13306034420170221 ) ) ;
#8503 = AXIS2_PLACEMENT_3D ( 'NONE', #1016, #7694, #12531 ) ;
#8504 = DIRECTION ( 'NONE',  ( 0.000000000000000000, 1.000000000000000000, 0.000000000000000000 ) ) ;
#8505 = CARTESIAN_POINT ( 'NONE',  ( 5.000000000000000000, 15.61693798565496394, 61.03368945066441142 ) ) ;
#8506 = VERTEX_POINT ( 'NONE', #7796 ) ;
#8507 = CARTESIAN_POINT ( 'NONE',  ( -4.000000000000000000, 0.7924765000094600165, -0.05906175389889745803 ) ) ;
#8508 = ORIENTED_EDGE ( 'NONE', *, *, #10959, .F. ) ;
#8509 = DIRECTION ( 'NONE',  ( 0.000000000000000000, 0.3090169943749411785, 0.9510565162951555296 ) ) ;
#8510 = LINE ( 'NONE', #5835, #11180 ) ;
#8511 = EDGE_LOOP ( 'NONE', ( #916, #9093, #16933, #3473 ) ) ;
#8512 = APPLICATION_PROTOCOL_DEFINITION ( 'draft international standard', 'automotive_design', 1998, #17652 ) ;
#8513 = LINE ( 'NONE', #11177, #5378 ) ;
#8514 = EDGE_LOOP ( 'NONE', ( #7348, #8850, #12294, #12989 ) ) ;
#8515 = AXIS2_PLACEMENT_3D ( 'NONE', #928, #15580, #16916 ) ;
#8516 = CIRCLE ( 'NONE', #10645, 12.00000000001200284 ) ;
#8517 = CARTESIAN_POINT ( 'NONE',  ( 10.00000000000000000, -26.45033635316118747, 36.40576474687271258 ) ) ;
#8518 = CARTESIAN_POINT ( 'NONE',  ( 10.04305231718605285, -34.99999999999999289, -33.55933677959240669 ) ) ;
#8519 = CARTESIAN_POINT ( 'NONE',  ( -4.000000000000000000, -2.309401076758512694, -5.000000000000000000 ) ) ;
#8520 = CARTESIAN_POINT ( 'NONE',  ( 0.000000000000000000, 0.000000000000000000, 0.000000000000000000 ) ) ;
#8521 = DIRECTION ( 'NONE',  ( 0.000000000000000000, 1.000000000000000000, 0.000000000000000000 ) ) ;
#8522 = ORIENTED_EDGE ( 'NONE', *, *, #5696, .T. ) ;
#8523 = ADVANCED_FACE ( 'NONE', ( #16761 ), #9511, .T. ) ;
#8524 = EDGE_CURVE ( 'NONE', #9159, #16722, #7864, .T. ) ;
#8525 = CARTESIAN_POINT ( 'NONE',  ( 10.00000000000000000, 0.000000000000000000, 0.000000000000000000 ) ) ;
#8526 = DIRECTION ( 'NONE',  ( 0.000000000000000000, -1.000000000000000000, 0.000000000000000000 ) ) ;
#8527 = CARTESIAN_POINT ( 'NONE',  ( 10.00000000000000000, 27.72801475327282361, -5.086963483077305170 ) ) ;
#8528 = ORIENTED_EDGE ( 'NONE', *, *, #8714, .T. ) ;
#8529 = EDGE_LOOP ( 'NONE', ( #6971, #4771, #12391, #4085, #12417, #9931, #8528 ) ) ;
#8530 = AXIS2_PLACEMENT_3D ( 'NONE', #17016, #12814, #3965 ) ;
#8531 = CARTESIAN_POINT ( 'NONE',  ( 13.90576474687299680, 10.00000000000000000, 42.79754323328179311 ) ) ;
#8532 =( GEOMETRIC_REPRESENTATION_CONTEXT ( 3 ) GLOBAL_UNCERTAINTY_ASSIGNED_CONTEXT ( ( #13963 ) ) GLOBAL_UNIT_ASSIGNED_CONTEXT ( ( #4785, #10596, #3458 ) ) REPRESENTATION_CONTEXT ( 'NONE', 'WORKASPACE' ) );
#8533 =( NAMED_UNIT ( * ) PLANE_ANGLE_UNIT ( ) SI_UNIT ( $, .RADIAN. ) );
#8534 = ADVANCED_FACE ( 'NONE', ( #13622 ), #18181, .F. ) ;
#8535 = ORIENTED_EDGE ( 'NONE', *, *, #1328, .T. ) ;
#8536 = DIRECTION ( 'NONE',  ( 1.000000000000000000, 0.000000000000000000, 0.000000000000000000 ) ) ;
#8537 = EDGE_CURVE ( 'NONE', #17827, #8441, #1192, .T. ) ;
#8538 = DIRECTION ( 'NONE',  ( 0.000000000000000000, 1.000000000000000000, 3.491481338843133355E-15 ) ) ;
#8539 = ADVANCED_FACE ( 'NONE', ( #12366 ), #956, .F. ) ;
#8540 = DIRECTION ( 'NONE',  ( 1.000000000000000000, -0.000000000000000000, 0.000000000000000000 ) ) ;
#8541 = ORIENTED_EDGE ( 'NONE', *, *, #4742, .T. ) ;
#8543 = CIRCLE ( 'NONE', #17377, 12.00000000001200462 ) ;
#8542 = CARTESIAN_POINT ( 'NONE',  ( 10.00000000000000000, 61.47135697633797946, -13.79392154159067196 ) ) ;
#8544 = EDGE_LOOP ( 'NONE', ( #17685, #4046, #13661, #17051 ) ) ;
#8545 = DIRECTION ( 'NONE',  ( -1.000000000000000000, -0.000000000000000000, -0.000000000000000000 ) ) ;
#8546 = EDGE_LOOP ( 'NONE', ( #1603, #7960, #10750, #6371 ) ) ;
#8547 = LINE ( 'NONE', #12931, #17490 ) ;
#8549 = ORIENTED_EDGE ( 'NONE', *, *, #379, .F. ) ;
#8548 = EDGE_CURVE ( 'NONE', #3664, #16857, #10606, .T. ) ;
#8550 = EDGE_CURVE ( 'NONE', #944, #4267, #3799, .T. ) ;
#8551 = CARTESIAN_POINT ( 'NONE',  ( 4.999999999999999112, -4.007856633823834613, 62.87238730325619684 ) ) ;
#8552 = DIRECTION ( 'NONE',  ( 0.000000000000000000, 0.000000000000000000, 1.000000000000000000 ) ) ;
#8553 = ORIENTED_EDGE ( 'NONE', *, *, #17106, .F. ) ;
#8554 = ORIENTED_EDGE ( 'NONE', *, *, #935, .T. ) ;
#8555 = CYLINDRICAL_SURFACE ( 'NONE', #4175, 33.00000000003299760 ) ;
#8556 = EDGE_CURVE ( 'NONE', #5984, #3048, #5131, .T. ) ;
#8557 = ORIENTED_EDGE ( 'NONE', *, *, #9581, .T. ) ;
#8558 = DIRECTION ( 'NONE',  ( 0.000000000000000000, 0.000000000000000000, 1.000000000000000000 ) ) ;
#8559 = DIRECTION ( 'NONE',  ( 0.000000000000000000, 0.9510565162951545304, -0.3090169943749446202 ) ) ;
#8560 = EDGE_CURVE ( 'NONE', #2359, #16326, #2369, .T. ) ;
#8561 = CIRCLE ( 'NONE', #13725, 24.00000000002399503 ) ;
#8562 = EDGE_CURVE ( 'NONE', #16785, #17588, #2181, .T. ) ;
#8563 = CARTESIAN_POINT ( 'NONE',  ( 5.200000000000002842, 0.000000000000000000, 0.000000000000000000 ) ) ;
#8564 = EDGE_LOOP ( 'NONE', ( #9795, #4795, #4624, #978 ) ) ;
#8565 = ORIENTED_EDGE ( 'NONE', *, *, #13530, .F. ) ;
#8566 = DIRECTION ( 'NONE',  ( -1.000000000000000000, 0.000000000000000000, 0.000000000000000000 ) ) ;
#8567 = DIRECTION ( 'NONE',  ( 0.000000000000000000, 0.000000000000000000, -1.000000000000000000 ) ) ;
#8568 = DIRECTION ( 'NONE',  ( 0.000000000000000000, 0.000000000000000000, 1.000000000000000000 ) ) ;
#8569 = LINE ( 'NONE', #4292, #12373 ) ;
#8570 = DIRECTION ( 'NONE',  ( 0.000000000000000000, 0.4999999999999991118, -0.8660254037844391517 ) ) ;
#8571 = LINE ( 'NONE', #5237, #12540 ) ;
#8572 = LINE ( 'NONE', #18378, #12345 ) ;
#8573 = ORIENTED_EDGE ( 'NONE', *, *, #10399, .T. ) ;
#8574 = CARTESIAN_POINT ( 'NONE',  ( 5.000000000000000000, 29.03656532225563680, 15.68049343256006800 ) ) ;
#8575 = SURFACE_STYLE_USAGE ( .BOTH. , #16001 ) ;
#8576 = VECTOR ( 'NONE', #11995, 1000.000000000000000 ) ;
#8577 = ORIENTED_EDGE ( 'NONE', *, *, #15893, .F. ) ;
#8578 = DIRECTION ( 'NONE',  ( 0.000000000000000000, -0.1564344650402381964, 0.9876883405951365491 ) ) ;
#8579 = CARTESIAN_POINT ( 'NONE',  ( 12.49999999999999289, 0.000000000000000000, -27.00000000000000000 ) ) ;
#8580 = EDGE_CURVE ( 'NONE', #15091, #5686, #9704, .T. ) ;
#8581 = ORIENTED_EDGE ( 'NONE', *, *, #2944, .F. ) ;
#8582 = VERTEX_POINT ( 'NONE', #13997 ) ;
#8583 = DIRECTION ( 'NONE',  ( 1.000000000000000000, 0.000000000000000000, 0.000000000000000000 ) ) ;
#8584 = CARTESIAN_POINT ( 'NONE',  ( 10.00000000000000000, 0.000000000000000000, 0.000000000000000000 ) ) ;
#8585 = ORIENTED_EDGE ( 'NONE', *, *, #17782, .F. ) ;
#8586 = DIRECTION ( 'NONE',  ( 0.000000000000000000, 0.000000000000000000, 1.000000000000000000 ) ) ;
#8587 = CARTESIAN_POINT ( 'NONE',  ( 4.000000000000000000, 2.309401076758515803, -0.4999999999999995559 ) ) ;
#8588 = DIRECTION ( 'NONE',  ( 0.000000000000000000, 0.4539904997395412534, 0.8910065241883706744 ) ) ;
#8589 = CARTESIAN_POINT ( 'NONE',  ( 5.200000000000002842, 0.000000000000000000, 0.000000000000000000 ) ) ;
#8590 = DIRECTION ( 'NONE',  ( 0.01644736842105263414, 0.9998647328874152862, -0.000000000000000000 ) ) ;
#8591 = ORIENTED_EDGE ( 'NONE', *, *, #12638, .T. ) ;
#8592 = DIRECTION ( 'NONE',  ( -1.000000000000000000, -0.000000000000000000, -0.000000000000000000 ) ) ;
#8593 = ORIENTED_EDGE ( 'NONE', *, *, #1231, .T. ) ;
#8594 = ADVANCED_FACE ( 'NONE', ( #10660 ), #1987, .T. ) ;
#8595 = PRODUCT ( 'socket head cap screw_iso_ISO 4762 M5 x 30 - 22N', 'socket head cap screw_iso_ISO 4762 M5 x 30 - 22N', '', ( #2797 ) ) ;
#8596 = PRESENTATION_STYLE_ASSIGNMENT (( #2794 ) ) ;
#8597 = CARTESIAN_POINT ( 'NONE',  ( 0.000000000000000000, 0.000000000000000000, -5.000000000000000000 ) ) ;
#8598 = ORIENTED_EDGE ( 'NONE', *, *, #16836, .T. ) ;
#8599 = EDGE_CURVE ( 'NONE', #5775, #16191, #1671, .T. ) ;
#8600 = SHAPE_DEFINITION_REPRESENTATION ( #1761, #1770 ) ;
#8601 = VECTOR ( 'NONE', #10282, 1000.000000000000000 ) ;
#8602 = CARTESIAN_POINT ( 'NONE',  ( 10.04305231718579705, -34.99999999999999289, 33.55933677959249195 ) ) ;
#8603 = ORIENTED_EDGE ( 'NONE', *, *, #4568, .T. ) ;
#8604 = AXIS2_PLACEMENT_3D ( 'NONE', #18396, #15555, #2502 ) ;
#8605 = AXIS2_PLACEMENT_3D ( 'NONE', #16005, #3148, #5728 ) ;
#8606 = VERTEX_POINT ( 'NONE', #17993 ) ;
#8607 = DIRECTION ( 'NONE',  ( -1.000000000000000000, 0.000000000000000000, -0.000000000000000000 ) ) ;
#8608 = DIRECTION ( 'NONE',  ( 0.000000000000000000, -1.000000000000000000, 0.000000000000000000 ) ) ;
#8609 = DIRECTION ( 'NONE',  ( 0.000000000000000000, 0.4999999999999991118, -0.8660254037844391517 ) ) ;
#8610 = EDGE_CURVE ( 'NONE', #2365, #15687, #17333, .T. ) ;
#8611 = DIRECTION ( 'NONE',  ( -1.000000000000000000, 0.000000000000000000, 0.000000000000000000 ) ) ;
#8612 = AXIS2_PLACEMENT_3D ( 'NONE', #13591, #16448, #9005 ) ;
#8613 = VECTOR ( 'NONE', #14955, 1000.000000000000000 ) ;
#8614 = DIRECTION ( 'NONE',  ( -1.000000000000000000, 0.000000000000000000, 0.000000000000000000 ) ) ;
#8615 = ORIENTED_EDGE ( 'NONE', *, *, #14737, .T. ) ;
#8616 = EDGE_CURVE ( 'NONE', #1945, #15342, #6380, .T. ) ;
#8617 = FACE_OUTER_BOUND ( 'NONE', #3541, .T. ) ;
#8618 = DIRECTION ( 'NONE',  ( 0.000000000000000000, -0.5000000000000009992, -0.8660254037844380415 ) ) ;
#8619 = DIRECTION ( 'NONE',  ( -1.000000000000000000, 0.000000000000000000, -0.000000000000000000 ) ) ;
#8620 = VERTEX_POINT ( 'NONE', #12275 ) ;
#8621 = ORIENTED_EDGE ( 'NONE', *, *, #16561, .F. ) ;
#8622 = DIRECTION ( 'NONE',  ( 0.000000000000000000, -0.000000000000000000, -1.000000000000000000 ) ) ;
#8623 = ORIENTED_EDGE ( 'NONE', *, *, #9706, .T. ) ;
#8624 = DIRECTION ( 'NONE',  ( 0.000000000000000000, 0.000000000000000000, -1.000000000000000000 ) ) ;
#8625 = EDGE_CURVE ( 'NONE', #12639, #2269, #16764, .T. ) ;
#8626 = CYLINDRICAL_SURFACE ( 'NONE', #10270, 56.24900000005625600 ) ;
#8627 = ORIENTED_EDGE ( 'NONE', *, *, #17736, .T. ) ;
#8628 = CARTESIAN_POINT ( 'NONE',  ( -2.595115354961444076, -7.673029147243174641, -1.000000000000000000 ) ) ;
#8629 = EDGE_CURVE ( 'NONE', #8023, #15168, #15498, .T. ) ;
#8630 = ORIENTED_EDGE ( 'NONE', *, *, #3078, .F. ) ;
#8631 = FACE_BOUND ( 'NONE', #2747, .T. ) ;
#8632 = VERTEX_POINT ( 'NONE', #18652 ) ;
#8633 = DIRECTION ( 'NONE',  ( -0.000000000000000000, -1.000000000000000000, -0.000000000000000000 ) ) ;
#8634 = ORIENTED_EDGE ( 'NONE', *, *, #4185, .F. ) ;
#8635 = COLOUR_RGB ( '',0.8941176470588234615, 0.8941176470588234615, 0.8941176470588234615 ) ;
#8636 = CARTESIAN_POINT ( 'NONE',  ( 0.000000000000000000, -58.55669782892444886, -23.24033432160500823 ) ) ;
#8637 = DIRECTION ( 'NONE',  ( -1.000000000000000000, -0.000000000000000000, -0.000000000000000000 ) ) ;
#8638 = ORIENTED_EDGE ( 'NONE', *, *, #4241, .F. ) ;
#8639 = ORIENTED_EDGE ( 'NONE', *, *, #12620, .F. ) ;
#8640 = DIRECTION ( 'NONE',  ( 0.000000000000000000, 0.000000000000000000, -1.000000000000000000 ) ) ;
#8641 = ORIENTED_EDGE ( 'NONE', *, *, #8067, .T. ) ;
#8642 = DIRECTION ( 'NONE',  ( 0.000000000000000000, 0.000000000000000000, 1.000000000000000000 ) ) ;
#8643 = EDGE_CURVE ( 'NONE', #243, #16476, #5456, .T. ) ;
#8644 = EDGE_CURVE ( 'NONE', #17183, #9889, #12762, .T. ) ;
#8645 = COLOUR_RGB ( '',1.000000000000000000, 0.9490196078431372140, 0.9098039215686274384 ) ;
#8646 = CARTESIAN_POINT ( 'NONE',  ( 10.00000000000000000, -26.20671763660627462, -1.489278925039791535 ) ) ;
#8647 = EDGE_CURVE ( 'NONE', #17978, #13907, #9890, .T. ) ;
#8648 = ADVANCED_FACE ( 'NONE', ( #12939 ), #5606, .T. ) ;
#8649 = ORIENTED_EDGE ( 'NONE', *, *, #1098, .T. ) ;
#8650 = EDGE_CURVE ( 'NONE', #11456, #16890, #18530, .T. ) ;
#8651 = ORIENTED_EDGE ( 'NONE', *, *, #6208, .T. ) ;
#8652 = CARTESIAN_POINT ( 'NONE',  ( -90.00000000009001155, 1.000000000000014655, -1.301042606982603940E-15 ) ) ;
#8653 = CARTESIAN_POINT ( 'NONE',  ( 3.061616997868383043E-15, -30.00000000000000000, -25.00000000000000000 ) ) ;
#8654 = DIRECTION ( 'NONE',  ( -1.000000000000000000, -0.000000000000000000, -0.000000000000000000 ) ) ;
#8655 = CARTESIAN_POINT ( 'NONE',  ( 10.04305231718579705, -26.50000000000000000, 33.55933677959249195 ) ) ;
#8656 = FACE_OUTER_BOUND ( 'NONE', #11886, .T. ) ;
#8657 = DIRECTION ( 'NONE',  ( -1.000000000000000000, -0.000000000000000000, 0.000000000000000000 ) ) ;
#8658 = CARTESIAN_POINT ( 'NONE',  ( 10.00000000000000000, -1.017308535511979972, -56.37237871411034718 ) ) ;
#8659 = EDGE_CURVE ( 'NONE', #14764, #4178, #11319, .T. ) ;
#8660 = FACE_BOUND ( 'NONE', #1126, .T. ) ;
#8661 = VERTEX_POINT ( 'NONE', #14447 ) ;
#8662 = CARTESIAN_POINT ( 'NONE',  ( 0.000000000000000000, -1.489278925039337675, -26.20671763660630305 ) ) ;
#8663 = DIRECTION ( 'NONE',  ( 1.000000000000000000, 0.000000000000000000, 0.000000000000000000 ) ) ;
#8664 = EDGE_CURVE ( 'NONE', #7319, #9233, #8495, .T. ) ;
#8665 = ORIENTED_EDGE ( 'NONE', *, *, #18298, .F. ) ;
#8666 = LINE ( 'NONE', #18588, #4509 ) ;
#8667 = DIRECTION ( 'NONE',  ( -0.000000000000000000, -1.000000000000000000, -0.000000000000000000 ) ) ;
#8668 = AXIS2_PLACEMENT_3D ( 'NONE', #3326, #15026, #3219 ) ;
#8669 = CIRCLE ( 'NONE', #12627, 25.00000000000000000 ) ;
#8670 = ORIENTED_EDGE ( 'NONE', *, *, #11534, .F. ) ;
#8671 = EDGE_CURVE ( 'NONE', #1723, #3100, #2557, .T. ) ;
#8672 = ORIENTED_EDGE ( 'NONE', *, *, #16492, .T. ) ;
#8673 = PRODUCT_DEFINITION_FORMATION_WITH_SPECIFIED_SOURCE ( 'ANY', '', #6337, .NOT_KNOWN. ) ;
#8674 = DIRECTION ( 'NONE',  ( 0.000000000000000000, -0.5877852522924804646, 0.8090169943749421222 ) ) ;
#8675 = DIRECTION ( 'NONE',  ( 0.000000000000000000, 0.000000000000000000, -1.000000000000000000 ) ) ;
#8676 = AXIS2_PLACEMENT_3D ( 'NONE', #8814, #13114, #10149 ) ;
#8677 = ORIENTED_EDGE ( 'NONE', *, *, #964, .T. ) ;
#8678 = TOROIDAL_SURFACE ( 'NONE', #2286, 29.90000000000000213, 0.1000000000000028644 ) ;
#8679 = EDGE_CURVE ( 'NONE', #4486, #4831, #10082, .T. ) ;
#8680 = DIRECTION ( 'NONE',  ( 1.000000000000000000, 0.000000000000000000, 0.000000000000000000 ) ) ;
#8681 = LINE ( 'NONE', #13076, #5711 ) ;
#8682 = DIRECTION ( 'NONE',  ( 0.000000000000000000, 0.000000000000000000, 1.000000000000000000 ) ) ;
#8683 = CARTESIAN_POINT ( 'NONE',  ( 5.000000000000000000, 22.76987570971561681, -23.88582760061456511 ) ) ;
#8684 = VERTEX_POINT ( 'NONE', #18468 ) ;
#8685 = FACE_OUTER_BOUND ( 'NONE', #6570, .T. ) ;
#8686 = ORIENTED_EDGE ( 'NONE', *, *, #11792, .F. ) ;
#8687 = DIRECTION ( 'NONE',  ( -1.000000000000000000, 0.000000000000000000, -0.000000000000000000 ) ) ;
#8688 = LINE ( 'NONE', #4321, #10890 ) ;
#8689 = ORIENTED_EDGE ( 'NONE', *, *, #3264, .F. ) ;
#8690 = AXIS2_PLACEMENT_3D ( 'NONE', #7875, #7492, #261 ) ;
#8691 = ITEM_DEFINED_TRANSFORMATION ( 'NONE', 'NONE', #13821,  #8017 ) ;
#8692 = VERTEX_POINT ( 'NONE', #2756 ) ;
#8693 = AXIS2_PLACEMENT_3D ( 'NONE', #3695, #12452, #11007 ) ;
#8694 = VECTOR ( 'NONE', #10395, 1000.000000000000000 ) ;
#8695 = DIRECTION ( 'NONE',  ( 0.000000000000000000, 0.000000000000000000, 1.000000000000000000 ) ) ;
#8696 = DIRECTION ( 'NONE',  ( -1.000000000000000000, 0.000000000000000000, 0.000000000000000000 ) ) ;
#8697 = AXIS2_PLACEMENT_3D ( 'NONE', #18128, #811, #8237 ) ;
#8698 = CARTESIAN_POINT ( 'NONE',  ( 10.00000000000000000, 0.000000000000000000, 0.000000000000000000 ) ) ;
#8699 = EDGE_CURVE ( 'NONE', #10072, #2652, #14085, .T. ) ;
#8700 = CARTESIAN_POINT ( 'NONE',  ( 10.00000000000000000, 0.000000000000000000, 0.000000000000000000 ) ) ;
#8701 = CIRCLE ( 'NONE', #18439, 63.00000000006298961 ) ;
#8702 = CIRCLE ( 'NONE', #201, 56.24900000005625600 ) ;
#8703 = DIRECTION ( 'NONE',  ( 0.000000000000000000, 0.000000000000000000, 1.000000000000000000 ) ) ;
#8704 = AXIS2_PLACEMENT_3D ( 'NONE', #2479, #2675, #12576 ) ;
#8705 = VERTEX_POINT ( 'NONE', #12657 ) ;
#8706 = CARTESIAN_POINT ( 'NONE',  ( 0.000000000000000000, 18.64666490672447097, -53.06836994729213330 ) ) ;
#8707 = DIRECTION ( 'NONE',  ( 0.000000000000000000, -0.8090169943749402348, -0.5877852522924830181 ) ) ;
#8708 = CARTESIAN_POINT ( 'NONE',  ( 5.000000000000004441, 0.000000000000000000, 4.250000000000000000 ) ) ;
#8709 = VERTEX_POINT ( 'NONE', #15892 ) ;
#8710 = ORIENTED_EDGE ( 'NONE', *, *, #15790, .T. ) ;
#8711 = DIRECTION ( 'NONE',  ( 0.000000000000000000, -1.000000000000000000, 0.000000000000000000 ) ) ;
#8712 = EDGE_LOOP ( 'NONE', ( #11403, #9805, #2656, #3094 ) ) ;
#8713 = CIRCLE ( 'NONE', #2023, 56.24900000005626310 ) ;
#8714 = EDGE_CURVE ( 'NONE', #4170, #17591, #577, .T. ) ;
#8715 = CIRCLE ( 'NONE', #2028, 56.24900000005625600 ) ;
#8716 = CIRCLE ( 'NONE', #4165, 33.00000000003299760 ) ;
#8717 = AXIS2_PLACEMENT_3D ( 'NONE', #1424, #8568, #17343 ) ;
#8718 = ADVANCED_FACE ( 'NONE', ( #17056 ), #17335, .T. ) ;
#8719 = CARTESIAN_POINT ( 'NONE',  ( 0.000000000000000000, 0.000000000000000000, 0.000000000000000000 ) ) ;
#8720 = DIRECTION ( 'NONE',  ( -1.000000000000000000, -0.000000000000000000, -0.000000000000000000 ) ) ;
#8721 = DIRECTION ( 'NONE',  ( 0.000000000000000000, 0.000000000000000000, -1.000000000000000000 ) ) ;
#8722 = ORIENTED_EDGE ( 'NONE', *, *, #17068, .T. ) ;
#8723 = DIRECTION ( 'NONE',  ( 1.000000000000000000, 0.000000000000000000, 0.000000000000000000 ) ) ;
#8724 = AXIS2_PLACEMENT_3D ( 'NONE', #6261, #2500, #7322 ) ;
#8725 = ORIENTED_EDGE ( 'NONE', *, *, #2486, .T. ) ;
#8726 = CARTESIAN_POINT ( 'NONE',  ( 4.888507282057958925, -29.45674523562211888, -2.000000000000000000 ) ) ;
#8727 = ORIENTED_EDGE ( 'NONE', *, *, #18702, .F. ) ;
#8728 = EDGE_LOOP ( 'NONE', ( #319, #18492, #12844, #11674 ) ) ;
#8729 = DIRECTION ( 'NONE',  ( 0.000000000000000000, 0.000000000000000000, 1.000000000000000000 ) ) ;
#8730 = FACE_OUTER_BOUND ( 'NONE', #8977, .T. ) ;
#8731 = AXIS2_PLACEMENT_3D ( 'NONE', #9045, #4577, #12347 ) ;
#8732 = ORIENTED_EDGE ( 'NONE', *, *, #9650, .T. ) ;
#8733 = VERTEX_POINT ( 'NONE', #13039 ) ;
#8734 = VECTOR ( 'NONE', #15183, 1000.000000000000000 ) ;
#8735 = CYLINDRICAL_SURFACE ( 'NONE', #11768, 56.24900000005625600 ) ;
#8736 = VERTEX_POINT ( 'NONE', #5521 ) ;
#8737 = DIRECTION ( 'NONE',  ( -1.000000000000000000, -0.000000000000000000, -0.000000000000000000 ) ) ;
#8738 = CONICAL_SURFACE ( 'NONE', #6305, 4.000000000000000000, 0.8911886515913786111 ) ;
#8739 = FACE_OUTER_BOUND ( 'NONE', #12062, .T. ) ;
#8740 = CIRCLE ( 'NONE', #2068, 40.00000000000000000 ) ;
#8741 = EDGE_LOOP ( 'NONE', ( #4907, #488, #3404, #14730 ) ) ;
#8742 = PRODUCT ( 'needle roller bearing_nm_iso_ISO 3030 - 15C5060 - 26,SI,AC,26', 'needle roller bearing_nm_iso_ISO 3030 - 15C5060 - 26,SI,AC,26', '', ( #4234 ) ) ;
#8743 = ORIENTED_EDGE ( 'NONE', *, *, #4052, .T. ) ;
#8744 = LINE ( 'NONE', #11616, #13592 ) ;
#8745 = DIRECTION ( 'NONE',  ( 0.000000000000000000, 1.000000000000000000, 0.000000000000000000 ) ) ;
#8746 = PLANE ( 'NONE',  #5390 ) ;
#8747 = ORIENTED_EDGE ( 'NONE', *, *, #1305, .T. ) ;
#8748 = CYLINDRICAL_SURFACE ( 'NONE', #8140, 33.00000000003299760 ) ;
#8749 = CARTESIAN_POINT ( 'NONE',  ( 10.00000000000000000, 19.44239304137375868, 20.41355805489622455 ) ) ;
#8750 = DIRECTION ( 'NONE',  ( -1.000000000000000000, 0.000000000000000000, 0.000000000000000000 ) ) ;
#8751 = AXIS2_PLACEMENT_3D ( 'NONE', #11084, #12438, #16819 ) ;
#8752 = FACE_OUTER_BOUND ( 'NONE', #4726, .T. ) ;
#8753 = ORIENTED_EDGE ( 'NONE', *, *, #2535, .F. ) ;
#8754 = PLANE ( 'NONE',  #9729 ) ;
#8755 = EDGE_CURVE ( 'NONE', #10475, #2531, #3935, .T. ) ;
#8756 = ADVANCED_FACE ( 'NONE', ( #14179 ), #6946, .T. ) ;
#8757 = CARTESIAN_POINT ( 'NONE',  ( 0.000000000000000000, 27.94286728106398243, -3.730438010304017116 ) ) ;
#8758 = AXIS2_PLACEMENT_3D ( 'NONE', #1281, #1464, #14599 ) ;
#8759 = EDGE_CURVE ( 'NONE', #11810, #17358, #6840, .T. ) ;
#8760 = VERTEX_POINT ( 'NONE', #17501 ) ;
#8761 = CARTESIAN_POINT ( 'NONE',  ( -79.64793068852927149, -38.00000000000000000, 31.86039329588764701 ) ) ;
#8762 = FACE_BOUND ( 'NONE', #117, .T. ) ;
#8763 = AXIS2_PLACEMENT_3D ( 'NONE', #10223, #10325, #5765 ) ;
#8764 = AXIS2_PLACEMENT_3D ( 'NONE', #6854, #6961, #16776 ) ;
#8765 = ITEM_DEFINED_TRANSFORMATION ( 'NONE', 'NONE', #12633,  #8017 ) ;
#8766 = ADVANCED_FACE ( 'NONE', ( #14645 ), #15975, .F. ) ;
#8767 = EDGE_CURVE ( 'NONE', #1784, #10254, #16409, .T. ) ;
#8768 = AXIS2_PLACEMENT_3D ( 'NONE', #6809, #8248, #727 ) ;
#8769 = CIRCLE ( 'NONE', #2452, 20.00000000000000000 ) ;
#8770 = EDGE_LOOP ( 'NONE', ( #2020, #18450, #2961, #10023 ) ) ;
#8771 = AXIS2_PLACEMENT_3D ( 'NONE', #5727, #11544, #10105 ) ;
#8772 = DIRECTION ( 'NONE',  ( -0.000000000000000000, -1.000000000000000000, -0.000000000000000000 ) ) ;
#8773 = CARTESIAN_POINT ( 'NONE',  ( 10.00000000000000000, -26.71881558261766898, 49.49802920186213129 ) ) ;
#8774 = EDGE_CURVE ( 'NONE', #8186, #13820, #6051, .T. ) ;
#8775 = ORIENTED_EDGE ( 'NONE', *, *, #14780, .T. ) ;
#8776 = LINE ( 'NONE', #7340, #18196 ) ;
#8777 =( REPRESENTATION_RELATIONSHIP ('NONE','NONE', #11014, #2517 ) REPRESENTATION_RELATIONSHIP_WITH_TRANSFORMATION ( #10956 )SHAPE_REPRESENTATION_RELATIONSHIP( ) );
#8778 = LINE ( 'NONE', #13163, #1417 ) ;
#8779 = DIRECTION ( 'NONE',  ( 0.000000000000000000, 0.000000000000000000, 1.000000000000000000 ) ) ;
#8780 = CARTESIAN_POINT ( 'NONE',  ( 10.00000000000000000, 4.007856633823390524, 62.87238730325622527 ) ) ;
#8781 = LINE ( 'NONE', #13359, #8087 ) ;
#8782 = EDGE_LOOP ( 'NONE', ( #8133, #16516, #2493, #359 ) ) ;
#8783 = CYLINDRICAL_SURFACE ( 'NONE', #5455, 2.500000000000000444 ) ;
#8784 = VERTEX_POINT ( 'NONE', #7315 ) ;
#8785 = ADVANCED_FACE ( 'NONE', ( #17690 ), #5969, .T. ) ;
#8786 = ADVANCED_FACE ( 'NONE', ( #263 ), #10169, .T. ) ;
#8787 = DIRECTION ( 'NONE',  ( 0.000000000000000000, 0.000000000000000000, -1.000000000000000000 ) ) ;
#8788 = CARTESIAN_POINT ( 'NONE',  ( 0.000000000000000000, 24.33982105418901298, 50.71018745830453156 ) ) ;
#8789 = VECTOR ( 'NONE', #16508, 1000.000000000000000 ) ;
#8790 = ORIENTED_EDGE ( 'NONE', *, *, #1555, .F. ) ;
#8791 = VECTOR ( 'NONE', #5707, 1000.000000000000000 ) ;
#8792 = EDGE_LOOP ( 'NONE', ( #554, #4064, #14674, #11854 ) ) ;
#8793 = CIRCLE ( 'NONE', #3938, 63.00000000006298961 ) ;
#8794 = EDGE_CURVE ( 'NONE', #11271, #652, #12759, .T. ) ;
#8795 = CARTESIAN_POINT ( 'NONE',  ( 0.000000000000000000, -5.876895005581972420, -62.72529079327814117 ) ) ;
#8796 = DIRECTION ( 'NONE',  ( 0.000000000000000000, 0.000000000000000000, 1.000000000000000000 ) ) ;
#8797 = CIRCLE ( 'NONE', #10916, 24.00000000002399858 ) ;
#8798 = DIRECTION ( 'NONE',  ( -1.000000000000000000, 0.000000000000000000, -0.000000000000000000 ) ) ;
#8799 = CARTESIAN_POINT ( 'NONE',  ( 4.999999999999999112, -32.70783759231089505, 4.381479206522875813 ) ) ;
#8800 = CARTESIAN_POINT ( 'NONE',  ( -0.3208286057739654917, 4.433571671609680465, -0.3503314178412548774 ) ) ;
#8801 = CARTESIAN_POINT ( 'NONE',  ( 10.00000000000000000, -47.29147401531984229, 41.62350880771904826 ) ) ;
#8802 = CARTESIAN_POINT ( 'NONE',  ( 10.04305231718579705, -34.99999999999999289, 30.90933677959249337 ) ) ;
#8803 = ORIENTED_EDGE ( 'NONE', *, *, #12808, .F. ) ;
#8804 = DIRECTION ( 'NONE',  ( 0.000000000000000000, 1.000000000000000000, 0.000000000000000000 ) ) ;
#8805 = DIRECTION ( 'NONE',  ( -0.000000000000000000, 1.000000000000000000, 0.000000000000000000 ) ) ;
#8806 = DIRECTION ( 'NONE',  ( 0.000000000000000000, 0.000000000000000000, 1.000000000000000000 ) ) ;
#8807 = ORIENTED_EDGE ( 'NONE', *, *, #7356, .F. ) ;
#8808 = ORIENTED_EDGE ( 'NONE', *, *, #13401, .F. ) ;
#8809 = CARTESIAN_POINT ( 'NONE',  ( 0.000000000000000000, 0.000000000000000000, 0.000000000000000000 ) ) ;
#8810 = ORIENTED_EDGE ( 'NONE', *, *, #10356, .T. ) ;
#8811 = CIRCLE ( 'NONE', #6685, 56.24900000005625600 ) ;
#8812 = EDGE_CURVE ( 'NONE', #9886, #9496, #16079, .T. ) ;
#8813 = VECTOR ( 'NONE', #11373, 1000.000000000000000 ) ;
#8814 = CARTESIAN_POINT ( 'NONE',  ( 0.000000000000000000, 10.00000000000000000, 0.000000000000000000 ) ) ;
#8815 = DIRECTION ( 'NONE',  ( 0.000000000000000000, -0.5000000000000009992, -0.8660254037844380415 ) ) ;
#8816 = DIRECTION ( 'NONE',  ( -1.000000000000000000, 0.000000000000000000, -0.000000000000000000 ) ) ;
#8817 = ORIENTED_EDGE ( 'NONE', *, *, #4266, .F. ) ;
#8818 = LINE ( 'NONE', #1583, #6432 ) ;
#8819 = ORIENTED_EDGE ( 'NONE', *, *, #13791, .F. ) ;
#8820 = VECTOR ( 'NONE', #2717, 1000.000000000000000 ) ;
#8821 = CYLINDRICAL_SURFACE ( 'NONE', #15147, 2.649999999999999467 ) ;
#8822 = VERTEX_POINT ( 'NONE', #8834 ) ;
#8823 = ORIENTED_EDGE ( 'NONE', *, *, #5164, .F. ) ;
#8824 = VECTOR ( 'NONE', #7063, 999.9999999999998863 ) ;
#8825 = ADVANCED_FACE ( 'NONE', ( #87 ), #1785, .F. ) ;
#8826 = CARTESIAN_POINT ( 'NONE',  ( -90.40196296004810961, -10.00000000000001954, 6.951864913735149365 ) ) ;
#8827 = DIRECTION ( 'NONE',  ( 0.9995235871707960351, -0.03086419753086420970, 0.000000000000000000 ) ) ;
#8828 = EDGE_LOOP ( 'NONE', ( #10147, #1044 ) ) ;
#8829 = ORIENTED_EDGE ( 'NONE', *, *, #5736, .F. ) ;
#8830 = DIRECTION ( 'NONE',  ( 0.000000000000000000, 0.000000000000000000, 1.000000000000000000 ) ) ;
#8831 = EDGE_CURVE ( 'NONE', #9657, #9696, #3018, .T. ) ;
#8832 =( LENGTH_UNIT ( ) NAMED_UNIT ( * ) SI_UNIT ( .MILLI., .METRE. ) );
#8833 = EDGE_LOOP ( 'NONE', ( #10066, #14124, #7181 ) ) ;
#8834 = CARTESIAN_POINT ( 'NONE',  ( -26.29305231718584324, -26.50000000000000000, 16.45302069950530566 ) ) ;
#8835 = AXIS2_PLACEMENT_3D ( 'NONE', #3436, #12455, #477 ) ;
#8836 = ORIENTED_EDGE ( 'NONE', *, *, #8986, .T. ) ;
#8837 = ORIENTED_EDGE ( 'NONE', *, *, #18275, .F. ) ;
#8838 = DIRECTION ( 'NONE',  ( -1.000000000000000000, 0.000000000000000000, 0.000000000000000000 ) ) ;
#8839 = CARTESIAN_POINT ( 'NONE',  ( 0.2500000000000002220, 4.898587196589412829E-16, -4.000000000000000000 ) ) ;
#8840 = DIRECTION ( 'NONE',  ( -0.000000000000000000, 0.000000000000000000, -1.000000000000000000 ) ) ;
#8841 = EDGE_CURVE ( 'NONE', #6436, #15930, #16712, .T. ) ;
#8842 = ORIENTED_EDGE ( 'NONE', *, *, #13220, .T. ) ;
#8843 = DIRECTION ( 'NONE',  ( 0.000000000000000000, -1.000000000000000000, -1.040834085585043434E-14 ) ) ;
#8844 = CYLINDRICAL_SURFACE ( 'NONE', #11523, 12.00000000001200107 ) ;
#8845 = DIRECTION ( 'NONE',  ( 1.000000000000000000, 0.000000000000000000, 0.000000000000000000 ) ) ;
#8846 = DIRECTION ( 'NONE',  ( 0.000000000000000000, 0.5877852522924742473, -0.8090169943749465631 ) ) ;
#8847 = VERTEX_POINT ( 'NONE', #17776 ) ;
#8848 = CARTESIAN_POINT ( 'NONE',  ( -17.77999999999999758, 0.000000000000000000, 30.00000000000000711 ) ) ;
#8849 = CIRCLE ( 'NONE', #15548, 4.000000000000000000 ) ;
#8850 = ORIENTED_EDGE ( 'NONE', *, *, #13196, .F. ) ;
#8851 = CARTESIAN_POINT ( 'NONE',  ( 5.000000000000000000, 23.88582760061481380, 22.76987570971536101 ) ) ;
#8852 = DIRECTION ( 'NONE',  ( 2.220446049250313081E-16, 0.000000000000000000, 1.000000000000000000 ) ) ;
#8853 = VECTOR ( 'NONE', #2604, 1000.000000000000000 ) ;
#8854 = ADVANCED_FACE ( 'NONE', ( #7403 ), #357, .T. ) ;
#8855 = VERTEX_POINT ( 'NONE', #16362 ) ;
#8856 = DIRECTION ( 'NONE',  ( 0.000000000000000000, 0.5000000000000009992, 0.8660254037844380415 ) ) ;
#8857 = ADVANCED_FACE ( 'NONE', ( #1598 ), #13317, .T. ) ;
#8858 = DIRECTION ( 'NONE',  ( 1.000000000000000000, 0.000000000000000000, 0.000000000000000000 ) ) ;
#8859 = VERTEX_POINT ( 'NONE', #9116 ) ;
#8860 = DIRECTION ( 'NONE',  ( -1.000000000000000000, 0.000000000000000000, 0.000000000000000000 ) ) ;
#8861 = CARTESIAN_POINT ( 'NONE',  ( 0.2500000000000002220, 0.000000000000000000, 0.000000000000000000 ) ) ;
#8862 = CIRCLE ( 'NONE', #3715, 4.000000000000000000 ) ;
#8863 = PRODUCT_DEFINITION ( 'UNKNOWN', '', #5326, #12838 ) ;
#8864 = DIRECTION ( 'NONE',  ( 0.000000000000000000, 0.000000000000000000, 1.000000000000000000 ) ) ;
#8865 = DIRECTION ( 'NONE',  ( -1.000000000000000000, -0.000000000000000000, -0.000000000000000000 ) ) ;
#8866 = DIRECTION ( 'NONE',  ( -1.000000000000000000, -0.000000000000000000, -0.000000000000000000 ) ) ;
#8867 = VERTEX_POINT ( 'NONE', #3124 ) ;
#8868 = DIRECTION ( 'NONE',  ( -1.000000000000000000, 0.000000000000000000, 0.000000000000000000 ) ) ;
#8869 = EDGE_LOOP ( 'NONE', ( #17319, #16550, #5437, #8710 ) ) ;
#8870 =( LENGTH_UNIT ( ) NAMED_UNIT ( * ) SI_UNIT ( .MILLI., .METRE. ) );
#8871 = DIRECTION ( 'NONE',  ( 0.000000000000000000, 0.000000000000000000, 1.000000000000000000 ) ) ;
#8872 = ORIENTED_EDGE ( 'NONE', *, *, #4455, .T. ) ;
#8873 = SHAPE_DEFINITION_REPRESENTATION ( #4958, #5670 ) ;
#8874 = VERTEX_POINT ( 'NONE', #11609 ) ;
#8875 = EDGE_CURVE ( 'NONE', #79, #1653, #6070, .T. ) ;
#8876 = AXIS2_PLACEMENT_3D ( 'NONE', #7232, #15906, #16184 ) ;
#8877 = APPLICATION_CONTEXT ( 'automotive_design' ) ;
#8878 = ADVANCED_FACE ( 'NONE', ( #8922 ), #11697, .T. ) ;
#8879 = CYLINDRICAL_SURFACE ( 'NONE', #2016, 26.24900000002624978 ) ;
#8880 = EDGE_CURVE ( 'NONE', #10905, #3687, #10720, .T. ) ;
#8881 = CARTESIAN_POINT ( 'NONE',  ( 10.00000000000000000, 53.89344778774834310, -16.10733642026427148 ) ) ;
#8882 = CARTESIAN_POINT ( 'NONE',  ( -2.059999999999998721, 2.522772406243545965E-16, -0.3080913168122742518 ) ) ;
#8883 = LINE ( 'NONE', #13272, #11261 ) ;
#8884 = AXIS2_PLACEMENT_3D ( 'NONE', #339, #13391, #8559 ) ;
#8885 = EDGE_CURVE ( 'NONE', #6727, #18475, #14887, .T. ) ;
#8886 = DIRECTION ( 'NONE',  ( 0.000000000000000000, 0.000000000000000000, 1.000000000000000000 ) ) ;
#8887 = DIRECTION ( 'NONE',  ( -1.000000000000000000, -0.000000000000000000, 0.000000000000000000 ) ) ;
#8888 = CARTESIAN_POINT ( 'NONE',  ( -6.259644161404860030E-16, -4.618802153517027165, -3.433295621305388234 ) ) ;
#8889 = VERTEX_POINT ( 'NONE', #15219 ) ;
#8890 = EDGE_CURVE ( 'NONE', #7713, #10053, #12464, .T. ) ;
#8891 = AXIS2_PLACEMENT_3D ( 'NONE', #4277, #8827, #14442 ) ;
#8892 = DIRECTION ( 'NONE',  ( -1.000000000000000000, 0.000000000000000000, 0.000000000000000000 ) ) ;
#8893 = DIRECTION ( 'NONE',  ( 0.9938152567191714803, 0.000000000000000000, -0.1110460963393456596 ) ) ;
#8894 = AXIS2_PLACEMENT_3D ( 'NONE', #5846, #11660, #10228 ) ;
#8895 = DIRECTION ( 'NONE',  ( 0.000000000000000000, 0.000000000000000000, 1.000000000000000000 ) ) ;
#8896 = ORIENTED_EDGE ( 'NONE', *, *, #13816, .T. ) ;
#8897 = VERTEX_POINT ( 'NONE', #11004 ) ;
#8898 = DIRECTION ( 'NONE',  ( -1.000000000000000000, -0.000000000000000000, -0.000000000000000000 ) ) ;
#8899 =( LENGTH_UNIT ( ) NAMED_UNIT ( * ) SI_UNIT ( .MILLI., .METRE. ) );
#8900 = EDGE_CURVE ( 'NONE', #9845, #17362, #6640, .T. ) ;
#8901 = DIRECTION ( 'NONE',  ( -1.000000000000000000, 0.000000000000000000, -0.000000000000000000 ) ) ;
#8902 = VERTEX_POINT ( 'NONE', #9293 ) ;
#8903 = AXIS2_PLACEMENT_3D ( 'NONE', #10997, #2528, #12821 ) ;
#8904 = CYLINDRICAL_SURFACE ( 'NONE', #3217, 2.649999999999999467 ) ;
#8905 = CARTESIAN_POINT ( 'NONE',  ( 0.1481481481481481122, -4.797713218419819903, -1.000000000000000000 ) ) ;
#8906 = CIRCLE ( 'NONE', #1310, 63.00000000006298961 ) ;
#8907 = CARTESIAN_POINT ( 'NONE',  ( 10.00000000000000000, 56.23315539212690339, -1.335003989221823062 ) ) ;
#8908 = VERTEX_POINT ( 'NONE', #15302 ) ;
#8909 = CYLINDRICAL_SURFACE ( 'NONE', #17679, 24.00000000002400213 ) ;
#8910 = EDGE_LOOP ( 'NONE', ( #13124, #12837, #8686, #12057 ) ) ;
#8911 = DIRECTION ( 'NONE',  ( -1.000000000000000000, -0.000000000000000000, -0.000000000000000000 ) ) ;
#8912 = ORIENTED_EDGE ( 'NONE', *, *, #15062, .F. ) ;
#8913 = EDGE_CURVE ( 'NONE', #7210, #14803, #2072, .T. ) ;
#8914 = DIRECTION ( 'NONE',  ( 0.000000000000000000, 0.000000000000000000, 1.000000000000000000 ) ) ;
#8915 = CARTESIAN_POINT ( 'NONE',  ( -12.69999999999999929, 0.000000000000000000, 0.000000000000000000 ) ) ;
#8916 = VERTEX_POINT ( 'NONE', #8057 ) ;
#8917 = EDGE_LOOP ( 'NONE', ( #5311, #6220, #2831, #10317 ) ) ;
#8918 = CARTESIAN_POINT ( 'NONE',  ( 10.00000000000000000, -40.70683587897930522, -38.81885513160031564 ) ) ;
#8919 = FILL_AREA_STYLE ('',( #5705 ) ) ;
#8920 = CIRCLE ( 'NONE', #7401, 0.2500000000000002220 ) ;
#8921 = ORIENTED_EDGE ( 'NONE', *, *, #648, .T. ) ;
#8922 = FACE_OUTER_BOUND ( 'NONE', #8365, .T. ) ;
#8923 = DIRECTION ( 'NONE',  ( -0.000000000000000000, -1.000000000000000000, 0.000000000000000000 ) ) ;
#8924 = ORIENTED_EDGE ( 'NONE', *, *, #6208, .F. ) ;
#8925 = VERTEX_POINT ( 'NONE', #9577 ) ;
#8926 = FACE_OUTER_BOUND ( 'NONE', #9525, .T. ) ;
#8927 = CARTESIAN_POINT ( 'NONE',  ( 0.000000000000000000, -53.89344778774823652, 16.10733642026462675 ) ) ;
#8928 = DIRECTION ( 'NONE',  ( 0.000000000000000000, 0.000000000000000000, 1.000000000000000000 ) ) ;
#8929 = ORIENTED_EDGE ( 'NONE', *, *, #8755, .F. ) ;
#8930 = CARTESIAN_POINT ( 'NONE',  ( 10.00000000000000000, 58.55669782892493203, -23.24033432160376478 ) ) ;
#8931 = EDGE_CURVE ( 'NONE', #3758, #16169, #646, .T. ) ;
#8932 = CARTESIAN_POINT ( 'NONE',  ( 5.032868406504335645, -28.36021363089093938, 0.000000000000000000 ) ) ;
#8933 = CARTESIAN_POINT ( 'NONE',  ( 11.25000000000000000, 0.000000000000000000, 0.000000000000000000 ) ) ;
#8934 = DIRECTION ( 'NONE',  ( -1.000000000000000000, -0.000000000000000000, -0.000000000000000000 ) ) ;
#8935 = ORIENTED_EDGE ( 'NONE', *, *, #4492, .F. ) ;
#8936 = CARTESIAN_POINT ( 'NONE',  ( 10.00000000000000000, 0.000000000000000000, 0.000000000000000000 ) ) ;
#8937 = CARTESIAN_POINT ( 'NONE',  ( 10.00000000000000000, -24.79895094899250196, -13.40641754777691830 ) ) ;
#8938 = ORIENTED_EDGE ( 'NONE', *, *, #5464, .T. ) ;
#8939 = DIRECTION ( 'NONE',  ( 0.000000000000000000, -0.9876883405951359940, -0.1564344650402419989 ) ) ;
#8940 = FACE_BOUND ( 'NONE', #9910, .T. ) ;
#8941 =( GEOMETRIC_REPRESENTATION_CONTEXT ( 3 ) GLOBAL_UNCERTAINTY_ASSIGNED_CONTEXT ( ( #2743 ) ) GLOBAL_UNIT_ASSIGNED_CONTEXT ( ( #3690, #4725, #12060 ) ) REPRESENTATION_CONTEXT ( 'NONE', 'WORKASPACE' ) );
#8942 = ADVANCED_FACE ( 'NONE', ( #3405 ), #13599, .T. ) ;
#8943 = ORIENTED_EDGE ( 'NONE', *, *, #465, .T. ) ;
#8944 = ADVANCED_FACE ( 'NONE', ( #10915 ), #12250, .F. ) ;
#8945 = DIRECTION ( 'NONE',  ( 1.000000000000000000, 0.000000000000000000, 0.000000000000000000 ) ) ;
#8946 = DIRECTION ( 'NONE',  ( 0.000000000000000000, 0.000000000000000000, -1.000000000000000000 ) ) ;
#8947 = ORIENTED_EDGE ( 'NONE', *, *, #3196, .T. ) ;
#8948 = DIRECTION ( 'NONE',  ( 0.000000000000000000, 0.000000000000000000, -1.000000000000000000 ) ) ;
#8949 = AXIS2_PLACEMENT_3D ( 'NONE', #17476, #14625, #13573 ) ;
#8950 = CARTESIAN_POINT ( 'NONE',  ( -10.00000000000000000, 0.000000000000000000, 0.000000000000000000 ) ) ;
#8951 = DIRECTION ( 'NONE',  ( 0.000000000000000000, 1.000000000000000000, 0.000000000000000000 ) ) ;
#8952 = DIRECTION ( 'NONE',  ( 0.000000000000000000, -0.5877852522924623679, -0.8090169943749552228 ) ) ;
#8953 = ORIENTED_EDGE ( 'NONE', *, *, #15623, .F. ) ;
#8954 = DIRECTION ( 'NONE',  ( 0.000000000000000000, 1.000000000000000000, 0.000000000000000000 ) ) ;
#8955 = ORIENTED_EDGE ( 'NONE', *, *, #18010, .T. ) ;
#8956 = AXIS2_PLACEMENT_3D ( 'NONE', #3891, #1565, #7453 ) ;
#8957 = CYLINDRICAL_SURFACE ( 'NONE', #11191, 24.00000000002399858 ) ;
#8958 = EDGE_LOOP ( 'NONE', ( #4338, #9791, #3128, #8269, #16866 ) ) ;
#8959 = ORIENTED_EDGE ( 'NONE', *, *, #14658, .T. ) ;
#8960 = AXIS2_PLACEMENT_3D ( 'NONE', #9847, #14232, #15363 ) ;
#8961 = ORIENTED_EDGE ( 'NONE', *, *, #66, .T. ) ;
#8962 = AXIS2_PLACEMENT_3D ( 'NONE', #1763, #1580, #430 ) ;
#8963 = AXIS2_PLACEMENT_3D ( 'NONE', #5598, #11399, #14900 ) ;
#8964 = CARTESIAN_POINT ( 'NONE',  ( 0.000000000000000000, -17.25000000000000355, 27.50000000000000000 ) ) ;
#8965 = FACE_OUTER_BOUND ( 'NONE', #6756, .T. ) ;
#8966 = FACE_OUTER_BOUND ( 'NONE', #2931, .T. ) ;
#8967 = CARTESIAN_POINT ( 'NONE',  ( 0.000000000000000000, -46.27827401617427228, 31.97297851452409034 ) ) ;
#8968 = DIRECTION ( 'NONE',  ( -1.000000000000000000, 0.000000000000000000, 0.000000000000000000 ) ) ;
#8969 = CARTESIAN_POINT ( 'NONE',  ( 32.50000000000000000, -26.50000000000000000, 3.680389326632394941E-13 ) ) ;
#8970 = AXIS2_PLACEMENT_3D ( 'NONE', #9508, #1143, #8280 ) ;
#8971 = CARTESIAN_POINT ( 'NONE',  ( 0.000000000000000000, 13.79392154159134876, 61.47135697633785156 ) ) ;
#8972 = CARTESIAN_POINT ( 'NONE',  ( 10.00000000000000000, 14.19907017806900207, -22.07705612348824076 ) ) ;
#8973 = ORIENTED_EDGE ( 'NONE', *, *, #4649, .T. ) ;
#8974 = CARTESIAN_POINT ( 'NONE',  ( 10.00000000000000000, 0.000000000000000000, 0.000000000000000000 ) ) ;
#8975 = DIRECTION ( 'NONE',  ( -1.000000000000000000, -0.000000000000000000, -0.000000000000000000 ) ) ;
#8976 = CARTESIAN_POINT ( 'NONE',  ( 10.00000000000000000, -40.58063702438372644, 39.14194549634347453 ) ) ;
#8977 = EDGE_LOOP ( 'NONE', ( #5127, #5229, #13285, #14991 ) ) ;
#8978 = CIRCLE ( 'NONE', #786, 25.00000000000000000 ) ;
#8979 = EDGE_LOOP ( 'NONE', ( #3903, #8378, #15833, #9962 ) ) ;
#8980 = AXIS2_PLACEMENT_3D ( 'NONE', #3157, #10474, #391 ) ;
#8981 = ADVANCED_FACE ( 'NONE', ( #5003 ), #6252, .T. ) ;
#8982 = EDGE_CURVE ( 'NONE', #12688, #15712, #18059, .T. ) ;
#8983 = DIRECTION ( 'NONE',  ( 0.000000000000000000, 0.000000000000000000, 1.000000000000000000 ) ) ;
#8984 = DIRECTION ( 'NONE',  ( 6.123233995736766036E-17, -1.000000000000000000, 0.000000000000000000 ) ) ;
#8986 = EDGE_CURVE ( 'NONE', #8661, #9272, #2161, .T. ) ;
#8985 = DIRECTION ( 'NONE',  ( 0.000000000000000000, 0.000000000000000000, 1.000000000000000000 ) ) ;
#8987 = ORIENTED_EDGE ( 'NONE', *, *, #3061, .T. ) ;
#8988 = EDGE_CURVE ( 'NONE', #16740, #6043, #15201, .T. ) ;
#8989 = CIRCLE ( 'NONE', #17510, 24.00000000002399858 ) ;
#8990 = AXIS2_PLACEMENT_3D ( 'NONE', #15948, #5490, #4061 ) ;
#8991 = CARTESIAN_POINT ( 'NONE',  ( 10.00000000000000000, 55.74967257055894265, -7.478235706488370660 ) ) ;
#8992 = CARTESIAN_POINT ( 'NONE',  ( 10.00000000000000000, 0.000000000000000000, 0.000000000000000000 ) ) ;
#8993 = AXIS2_PLACEMENT_3D ( 'NONE', #13095, #14416, #9946 ) ;
#8994 = AXIS2_PLACEMENT_3D ( 'NONE', #11666, #5578, #13105 ) ;
#8996 = VECTOR ( 'NONE', #6086, 1000.000000000000000 ) ;
#8995 = DIRECTION ( 'NONE',  ( 0.000000000000000000, 0.8910065241883656784, 0.4539904997395510788 ) ) ;
#8997 = ORIENTED_EDGE ( 'NONE', *, *, #8629, .T. ) ;
#8998 = DIRECTION ( 'NONE',  ( 0.000000000000000000, 0.000000000000000000, -1.000000000000000000 ) ) ;
#8999 = EDGE_CURVE ( 'NONE', #15225, #5247, #16637, .T. ) ;
#9000 = VERTEX_POINT ( 'NONE', #12167 ) ;
#9001 = DIRECTION ( 'NONE',  ( 0.000000000000000000, 0.000000000000000000, 1.000000000000000000 ) ) ;
#9002 = VERTEX_POINT ( 'NONE', #6358 ) ;
#9003 = B_SPLINE_CURVE_WITH_KNOTS ( 'NONE', 3,
 ( #157, #3299, #11776, #4820, #1951, #13118 ),
 .UNSPECIFIED., .F., .F.,
 ( 4, 2, 4 ),
 ( 0.002365888236227995517, 0.003551327329835084114, 0.004736766423442172712 ),
 .UNSPECIFIED. ) ;
#9004 = CARTESIAN_POINT ( 'NONE',  ( 2.354826896168714434, -6.962563485461402024, -1.000000000000000000 ) ) ;
#9005 = DIRECTION ( 'NONE',  ( 0.000000000000000000, 0.000000000000000000, -1.000000000000000000 ) ) ;
#9006 = AXIS2_PLACEMENT_3D ( 'NONE', #1942, #17948, #17574 ) ;
#9007 = VERTEX_POINT ( 'NONE', #7967 ) ;
#9008 = VERTEX_POINT ( 'NONE', #17973 ) ;
#9009 = ADVANCED_FACE ( 'NONE', ( #4922 ), #6448, .T. ) ;
#9010 = CARTESIAN_POINT ( 'NONE',  ( 10.00000000000000000, -18.64666490672410148, 53.06836994729227541 ) ) ;
#9011 = VECTOR ( 'NONE', #3369, 1000.000000000000000 ) ;
#9012 = EDGE_LOOP ( 'NONE', ( #146, #7284, #13021, #15038 ) ) ;
#9013 = DIRECTION ( 'NONE',  ( 0.000000000000000000, 0.000000000000000000, 1.000000000000000000 ) ) ;
#9014 = VECTOR ( 'NONE', #3738, 1000.000000000000000 ) ;
#9015 = CIRCLE ( 'NONE', #12686, 63.00000000006298961 ) ;
#9016 =( REPRESENTATION_RELATIONSHIP ('NONE','NONE', #11014, #2517 ) REPRESENTATION_RELATIONSHIP_WITH_TRANSFORMATION ( #17529 )SHAPE_REPRESENTATION_RELATIONSHIP( ) );
#9017 = ADVANCED_FACE ( 'NONE', ( #15121 ), #13779, .T. ) ;
#9018 = DIRECTION ( 'NONE',  ( -1.000000000000000000, -0.000000000000000000, 0.000000000000000000 ) ) ;
#9019 = CIRCLE ( 'NONE', #6280, 24.00000000002399148 ) ;
#9020 = CIRCLE ( 'NONE', #5063, 56.24900000005625600 ) ;
#9021 = ORIENTED_EDGE ( 'NONE', *, *, #17230, .F. ) ;
#9022 = AXIS2_PLACEMENT_3D ( 'NONE', #15621, #3811, #12670 ) ;
#9023 = AXIS2_PLACEMENT_3D ( 'NONE', #3151, #13783, #9402 ) ;
#9024 = ORIENTED_EDGE ( 'NONE', *, *, #7254, .T. ) ;
#9025 = DIRECTION ( 'NONE',  ( -1.000000000000000000, 0.000000000000000000, 0.000000000000000000 ) ) ;
#9026 = CARTESIAN_POINT ( 'NONE',  ( 10.00000000000000000, -12.18267823974769293, 25.42247726998010648 ) ) ;
#9027 = CARTESIAN_POINT ( 'NONE',  ( -4.203833317240879275, -1.627343821129593859, -3.597273115243890818 ) ) ;
#9028 = VERTEX_POINT ( 'NONE', #12827 ) ;
#9029 = CARTESIAN_POINT ( 'NONE',  ( 10.00000000000000000, -41.62350880771954564, 47.29147401531940176 ) ) ;
#9030 = DIRECTION ( 'NONE',  ( -1.000000000000000000, 0.000000000000000000, 0.000000000000000000 ) ) ;
#9031 = CARTESIAN_POINT ( 'NONE',  ( -11.15000000000000391, 3.061616997868383043E-15, -25.00000000000000000 ) ) ;
#9032 = FACE_BOUND ( 'NONE', #12527, .T. ) ;
#9033 = ORIENTED_EDGE ( 'NONE', *, *, #16822, .F. ) ;
#9034 = DIRECTION ( 'NONE',  ( 0.000000000000000000, 0.000000000000000000, -1.000000000000000000 ) ) ;
#9035 = CARTESIAN_POINT ( 'NONE',  ( 10.00000000000000000, 53.89344778774812994, 16.10733642026502466 ) ) ;
#9036 = ORIENTED_EDGE ( 'NONE', *, *, #1391, .F. ) ;
#9037 = CARTESIAN_POINT ( 'NONE',  ( 0.000000000000000000, 0.000000000000000000, 0.000000000000000000 ) ) ;
#9038 = DIRECTION ( 'NONE',  ( 0.000000000000000000, 0.000000000000000000, 1.000000000000000000 ) ) ;
#9039 = CIRCLE ( 'NONE', #8724, 150.0000000000000000 ) ;
#9040 = AXIS2_PLACEMENT_3D ( 'NONE', #15034, #1978, #7784 ) ;
#9041 = AXIS2_PLACEMENT_3D ( 'NONE', #11955, #13490, #431 ) ;
#9042 = CIRCLE ( 'NONE', #18776, 23.50000000000001066 ) ;
#9043 = ADVANCED_FACE ( 'NONE', ( #14260 ), #6919, .T. ) ;
#9044 = ORIENTED_EDGE ( 'NONE', *, *, #10591, .F. ) ;
#9045 = CARTESIAN_POINT ( 'NONE',  ( 10.00000000000000000, 0.000000000000000000, 0.000000000000000000 ) ) ;
#9046 = CARTESIAN_POINT ( 'NONE',  ( 10.00000000000000000, 4.381479206522985059, 32.70783759231087373 ) ) ;
#9047 = CIRCLE ( 'NONE', #11791, 4.250000000000000000 ) ;
#9048 = VERTEX_POINT ( 'NONE', #3876 ) ;
#9049 = DIRECTION ( 'NONE',  ( 0.000000000000000000, 0.000000000000000000, 1.000000000000000000 ) ) ;
#9050 = FACE_BOUND ( 'NONE', #11713, .T. ) ;
#9051 = AXIS2_PLACEMENT_3D ( 'NONE', #237, #6324, #11941 ) ;
#9052 = FACE_OUTER_BOUND ( 'NONE', #12024, .T. ) ;
#9053 = DIRECTION ( 'NONE',  ( 0.000000000000000000, 0.000000000000000000, 1.000000000000000000 ) ) ;
#9054 = CARTESIAN_POINT ( 'NONE',  ( 5.000000000000000888, 0.000000000000000000, 0.000000000000000000 ) ) ;
#9055 = EDGE_LOOP ( 'NONE', ( #1662, #1441, #13237, #6355 ) ) ;
#9056 = VECTOR ( 'NONE', #6876, 1000.000000000000000 ) ;
#9057 = DIRECTION ( 'NONE',  ( 0.000000000000000000, -0.5877852522924804646, 0.8090169943749421222 ) ) ;
#9058 = ORIENTED_EDGE ( 'NONE', *, *, #5179, .T. ) ;
#9059 = EDGE_CURVE ( 'NONE', #10237, #12166, #7892, .T. ) ;
#9060 = PRODUCT_DEFINITION_SHAPE ( 'NONE', 'NONE',  #14453 ) ;
#9061 = CARTESIAN_POINT ( 'NONE',  ( 0.000000000000000000, 0.000000000000000000, 0.000000000000000000 ) ) ;
#9062 = DIRECTION ( 'NONE',  ( -1.000000000000000000, -0.000000000000000000, 0.000000000000000000 ) ) ;
#9063 = EDGE_LOOP ( 'NONE', ( #12229, #14549, #11000, #17618, #9282 ) ) ;
#9064 = EDGE_CURVE ( 'NONE', #3517, #17226, #5, .T. ) ;
#9065 = ORIENTED_EDGE ( 'NONE', *, *, #12, .T. ) ;
#9066 = AXIS2_PLACEMENT_3D ( 'NONE', #17681, #14724, #6350 ) ;
#9067 = AXIS2_PLACEMENT_3D ( 'NONE', #6970, #4021, #8578 ) ;
#9068 = ORIENTED_EDGE ( 'NONE', *, *, #2735, .F. ) ;
#9069 = CIRCLE ( 'NONE', #2097, 55.00000000000000000 ) ;
#9070 = VECTOR ( 'NONE', #12483, 1000.000000000000000 ) ;
#9071 = ORIENTED_EDGE ( 'NONE', *, *, #17454, .T. ) ;
#9072 = FACE_OUTER_BOUND ( 'NONE', #10678, .T. ) ;
#9073 = DIRECTION ( 'NONE',  ( 1.000000000000000000, 0.000000000000000000, 0.000000000000000000 ) ) ;
#9074 = CARTESIAN_POINT ( 'NONE',  ( 9.345251662538453630, -28.92794965710190525, -2.000000000000000000 ) ) ;
#9075 = DIRECTION ( 'NONE',  ( -0.000000000000000000, -1.000000000000000000, 0.000000000000000000 ) ) ;
#9076 = LINE ( 'NONE', #13744, #16957 ) ;
#9077 = CIRCLE ( 'NONE', #4517, 2.649999999999999467 ) ;
#9078 = DIRECTION ( 'NONE',  ( -1.000000000000000000, -0.000000000000000000, -0.000000000000000000 ) ) ;
#9079 = CARTESIAN_POINT ( 'NONE',  ( 10.00000000000000000, -55.51919907100644735, -9.823366686501268319 ) ) ;
#9080 = DIRECTION ( 'NONE',  ( -1.000000000000000000, 0.000000000000000000, -0.000000000000000000 ) ) ;
#9081 = ORIENTED_EDGE ( 'NONE', *, *, #4911, .T. ) ;
#9082 = AXIS2_PLACEMENT_3D ( 'NONE', #13521, #16004, #11815 ) ;
#9083 = DIRECTION ( 'NONE',  ( 1.000000000000000000, 0.000000000000000000, 0.000000000000000000 ) ) ;
#9084 = DIRECTION ( 'NONE',  ( 0.000000000000000000, 0.000000000000000000, 1.000000000000000000 ) ) ;
#9085 = CIRCLE ( 'NONE', #8484, 24.00000000002400569 ) ;
#9086 = AXIS2_PLACEMENT_3D ( 'NONE', #15901, #15988, #11420 ) ;
#9087 = VERTEX_POINT ( 'NONE', #15496 ) ;
#9088 = VERTEX_POINT ( 'NONE', #11296 ) ;
#9089 = CIRCLE ( 'NONE', #895, 2.649999999999999467 ) ;
#9090 = CARTESIAN_POINT ( 'NONE',  ( 10.00000000000000000, 33.71303790549275448, 53.22058882792208578 ) ) ;
#9091 = DIRECTION ( 'NONE',  ( 0.000000000000000000, -1.000000000000000000, 0.000000000000000000 ) ) ;
#9092 = DIRECTION ( 'NONE',  ( 0.000000000000000000, 0.000000000000000000, 1.000000000000000000 ) ) ;
#9093 = ORIENTED_EDGE ( 'NONE', *, *, #5622, .F. ) ;
#9094 = AXIS2_PLACEMENT_3D ( 'NONE', #2108, #15336, #6394 ) ;
#9095 = VECTOR ( 'NONE', #15704, 1000.000000000000114 ) ;
#9096 = DIRECTION ( 'NONE',  ( 1.000000000000000000, 0.000000000000000000, 0.000000000000000000 ) ) ;
#9097 = FACE_OUTER_BOUND ( 'NONE', #15059, .T. ) ;
#9098 = DIRECTION ( 'NONE',  ( -1.000000000000000000, 0.000000000000000000, 0.000000000000000000 ) ) ;
#9099 = ORIENTED_EDGE ( 'NONE', *, *, #16702, .T. ) ;
#9100 = EDGE_CURVE ( 'NONE', #6853, #3758, #18544, .T. ) ;
#9101 = CYLINDRICAL_SURFACE ( 'NONE', #9157, 12.00000000001200462 ) ;
#9102 = EDGE_CURVE ( 'NONE', #2539, #16873, #4858, .T. ) ;
#9103 = ORIENTED_EDGE ( 'NONE', *, *, #3601, .F. ) ;
#9104 = CARTESIAN_POINT ( 'NONE',  ( 10.00000000000000000, -46.20417134726153563, 32.31183295104756326 ) ) ;
#9105 = VERTEX_POINT ( 'NONE', #18631 ) ;
#9106 = ADVANCED_FACE ( 'NONE', ( #4163 ), #5585, .T. ) ;
#9107 = CARTESIAN_POINT ( 'NONE',  ( 5.200000000000002842, 0.000000000000000000, 0.000000000000000000 ) ) ;
#9108 = CARTESIAN_POINT ( 'NONE',  ( -10.00000000000000000, 0.000000000000000000, 0.000000000000000000 ) ) ;
#9109 = AXIS2_PLACEMENT_3D ( 'NONE', #3773, #9485, #9671 ) ;
#9110 = ORIENTED_EDGE ( 'NONE', *, *, #14480, .F. ) ;
#9111 = ORIENTED_EDGE ( 'NONE', *, *, #18205, .F. ) ;
#9112 = DIRECTION ( 'NONE',  ( -1.000000000000000000, -0.000000000000000000, -0.000000000000000000 ) ) ;
#9113 = PRESENTATION_LAYER_ASSIGNMENT (  '', '', ( #17339 ) ) ;
#9114 = EDGE_CURVE ( 'NONE', #4363, #13142, #17030, .T. ) ;
#9115 = ORIENTED_EDGE ( 'NONE', *, *, #154, .F. ) ;
#9116 = CARTESIAN_POINT ( 'NONE',  ( 10.00000000000000000, 56.23315539212690339, -1.335003989221823062 ) ) ;
#9117 = EDGE_CURVE ( 'NONE', #11652, #7353, #8261, .T. ) ;
#9118 = DIRECTION ( 'NONE',  ( 1.000000000000000000, 0.000000000000000000, 0.000000000000000000 ) ) ;
#9119 = AXIS2_PLACEMENT_3D ( 'NONE', #9569, #15385, #17024 ) ;
#9120 = VERTEX_POINT ( 'NONE', #3978 ) ;
#9121 = EDGE_CURVE ( 'NONE', #3414, #752, #17119, .T. ) ;
#9122 = AXIS2_PLACEMENT_3D ( 'NONE', #720, #12323, #16726 ) ;
#9123 = ADVANCED_FACE ( 'NONE', ( #2629 ), #8447, .T. ) ;
#9124 = ORIENTED_EDGE ( 'NONE', *, *, #4832, .F. ) ;
#9125 = DIRECTION ( 'NONE',  ( -0.9998850848853023665, 0.000000000000000000, -0.01515971714484241721 ) ) ;
#9126 = CARTESIAN_POINT ( 'NONE',  ( 130.0000000000000000, -30.00000000000000000, 125.0000000000000000 ) ) ;
#9127 = DIRECTION ( 'NONE',  ( 0.000000000000000000, 0.000000000000000000, -1.000000000000000000 ) ) ;
#9128 = VERTEX_POINT ( 'NONE', #9679 ) ;
#9129 = FACE_OUTER_BOUND ( 'NONE', #14186, .T. ) ;
#9130 = EDGE_CURVE ( 'NONE', #2059, #10049, #1509, .T. ) ;
#9131 = CARTESIAN_POINT ( 'NONE',  ( 4.799999999999999822, 0.000000000000000000, 0.000000000000000000 ) ) ;
#9132 = CARTESIAN_POINT ( 'NONE',  ( -94.77031323234206184, 1.821459649775647449E-14, 0.5330212624288541701 ) ) ;
#9133 = CARTESIAN_POINT ( 'NONE',  ( 5.000000000000000000, 47.29147401532013362, -41.62350880771872852 ) ) ;
#9134 = ORIENTED_EDGE ( 'NONE', *, *, #17857, .F. ) ;
#9135 = FACE_OUTER_BOUND ( 'NONE', #260, .T. ) ;
#9136 = EDGE_CURVE ( 'NONE', #2843, #12239, #6373, .T. ) ;
#9137 = DIRECTION ( 'NONE',  ( 0.000000000000000000, 0.000000000000000000, 1.000000000000000000 ) ) ;
#9138 = VERTEX_POINT ( 'NONE', #5397 ) ;
#9139 = CARTESIAN_POINT ( 'NONE',  ( 10.00000000000000000, -55.83748330407401284, 16.18620087215011338 ) ) ;
#9140 = CARTESIAN_POINT ( 'NONE',  ( 11.14999999999999680, 3.661693929450586610E-15, -29.90000000000000213 ) ) ;
#9141 = AXIS2_PLACEMENT_3D ( 'NONE', #17084, #11053, #16879 ) ;
#9142 = ORIENTED_EDGE ( 'NONE', *, *, #16328, .F. ) ;
#9143 = SURFACE_SIDE_STYLE ('',( #17804 ) ) ;
#9144 = ORIENTED_EDGE ( 'NONE', *, *, #12611, .F. ) ;
#9145 = DIRECTION ( 'NONE',  ( 0.000000000000000000, 0.000000000000000000, 1.000000000000000000 ) ) ;
#9146 = COLOUR_RGB ( '',0.8941176470588234615, 0.8941176470588234615, 0.8941176470588234615 ) ;
#9147 = DIRECTION ( 'NONE',  ( 0.000000000000000000, 0.000000000000000000, 1.000000000000000000 ) ) ;
#9148 = CARTESIAN_POINT ( 'NONE',  ( 13.90576474687263264, 0.000000000000000000, -45.44754323328189827 ) ) ;
#9149 = DIRECTION ( 'NONE',  ( 1.000000000000000000, 0.000000000000000000, 0.000000000000000000 ) ) ;
#9150 = VERTEX_POINT ( 'NONE', #9775 ) ;
#9151 = DIRECTION ( 'NONE',  ( 0.000000000000000000, 0.000000000000000000, 1.000000000000000000 ) ) ;
#9152 = ORIENTED_EDGE ( 'NONE', *, *, #12481, .F. ) ;
#9153 = EDGE_CURVE ( 'NONE', #10659, #5638, #7590, .T. ) ;
#9154 = CARTESIAN_POINT ( 'NONE',  ( 0.000000000000000000, -23.88582760061497368, 22.76987570971518338 ) ) ;
#9155 = ORIENTED_EDGE ( 'NONE', *, *, #4093, .T. ) ;
#9156 = ORIENTED_EDGE ( 'NONE', *, *, #714, .T. ) ;
#9157 = AXIS2_PLACEMENT_3D ( 'NONE', #17484, #11682, #14722 ) ;
#9158 = ORIENTED_EDGE ( 'NONE', *, *, #4637, .F. ) ;
#9159 = VERTEX_POINT ( 'NONE', #18306 ) ;
#9161 = DIRECTION ( 'NONE',  ( -1.000000000000000000, 0.000000000000000000, 0.000000000000000000 ) ) ;
#9160 = VECTOR ( 'NONE', #5556, 1000.000000000000000 ) ;
#9162 = CARTESIAN_POINT ( 'NONE',  ( 0.000000000000000000, 0.5192545390863916310, -1.000000000000000000 ) ) ;
#9163 = VECTOR ( 'NONE', #5132, 1000.000000000000000 ) ;
#9164 = CARTESIAN_POINT ( 'NONE',  ( 10.00000000000000000, -45.00825343884996954, -33.95787273855293620 ) ) ;
#9165 = CARTESIAN_POINT ( 'NONE',  ( 10.00000000000000000, 0.000000000000000000, 26.24900000002624978 ) ) ;
#9166 = CARTESIAN_POINT ( 'NONE',  ( 32.50000000000000000, -26.50000000000000000, 3.680389326632394941E-13 ) ) ;
#9167 = CARTESIAN_POINT ( 'NONE',  ( -10.00000000000000000, 0.000000000000000000, 0.000000000000000000 ) ) ;
#9168 = DIRECTION ( 'NONE',  ( 0.000000000000000000, -0.4539904997395351471, -0.8910065241883737830 ) ) ;
#9169 = ORIENTED_EDGE ( 'NONE', *, *, #16808, .T. ) ;
#9170 = DIRECTION ( 'NONE',  ( 0.000000000000000000, 0.000000000000000000, -1.000000000000000000 ) ) ;
#9171 = ORIENTED_EDGE ( 'NONE', *, *, #12856, .F. ) ;
#9172 = ADVANCED_FACE ( 'NONE', ( #9256 ), #3035, .T. ) ;
#9173 = DIRECTION ( 'NONE',  ( 0.000000000000000000, 0.4539904997395412534, 0.8910065241883705633 ) ) ;
#9174 = DIRECTION ( 'NONE',  ( -1.000000000000000000, -0.000000000000000000, 0.000000000000000000 ) ) ;
#9175 = DIRECTION ( 'NONE',  ( 0.000000000000000000, 0.000000000000000000, 1.000000000000000000 ) ) ;
#9176 = EDGE_LOOP ( 'NONE', ( #6672, #15778, #1089, #2947 ) ) ;
#9177 = ORIENTED_EDGE ( 'NONE', *, *, #11793, .F. ) ;
#9178 = CARTESIAN_POINT ( 'NONE',  ( -290.0000000000001705, -34.99999999999999289, 125.0000000000000000 ) ) ;
#9179 = DIRECTION ( 'NONE',  ( 0.000000000000000000, 0.000000000000000000, 1.000000000000000000 ) ) ;
#9180 = AXIS2_PLACEMENT_3D ( 'NONE', #14466, #2859, #15994 ) ;
#9181 = LINE ( 'NONE', #4529, #17694 ) ;
#9182 = VERTEX_POINT ( 'NONE', #16791 ) ;
#9183 = EDGE_CURVE ( 'NONE', #10830, #6436, #15349, .T. ) ;
#9184 = PLANE ( 'NONE',  #1092 ) ;
#9185 = CARTESIAN_POINT ( 'NONE',  ( -26.29305231718584324, -26.50000000000000000, 19.10302069950530779 ) ) ;
#9186 = DIRECTION ( 'NONE',  ( -0.000000000000000000, 1.000000000000000000, -0.000000000000000000 ) ) ;
#9187 = ORIENTED_EDGE ( 'NONE', *, *, #4405, .F. ) ;
#9188 = CARTESIAN_POINT ( 'NONE',  ( 1.317756351988342622, -3.857995168970215438, -0.04852650426602527628 ) ) ;
#9189 = EDGE_CURVE ( 'NONE', #380, #7033, #593, .T. ) ;
#9190 = ORIENTED_EDGE ( 'NONE', *, *, #17106, .T. ) ;
#9191 = UNCERTAINTY_MEASURE_WITH_UNIT (LENGTH_MEASURE( 1.000000000000000082E-05 ), #8172, 'distance_accuracy_value', 'NONE');
#9192 = DIRECTION ( 'NONE',  ( -1.000000000000000000, -0.000000000000000000, -0.000000000000000000 ) ) ;
#9193 = ORIENTED_EDGE ( 'NONE', *, *, #12800, .T. ) ;
#9194 = CARTESIAN_POINT ( 'NONE',  ( 0.000000000000000000, -61.47135697633769524, -13.79392154159200068 ) ) ;
#9195 = CARTESIAN_POINT ( 'NONE',  ( -0.5276280594146446346, 4.314175951381965746, -3.320322319201721495 ) ) ;
#9196 = ORIENTED_EDGE ( 'NONE', *, *, #1845, .T. ) ;
#9197 = VERTEX_POINT ( 'NONE', #12120 ) ;
#9198 = ADVANCED_BREP_SHAPE_REPRESENTATION ( '', ( #10108, #8017 ), #3161 ) ;
#9199 = LINE ( 'NONE', #8918, #11417 ) ;
#9200 = ORIENTED_EDGE ( 'NONE', *, *, #17985, .T. ) ;
#9201 = DIRECTION ( 'NONE',  ( 1.000000000000000000, 0.000000000000000000, 0.000000000000000000 ) ) ;
#9202 = AXIS2_PLACEMENT_3D ( 'NONE', #7488, #13309, #10257 ) ;
#9203 = EDGE_CURVE ( 'NONE', #7581, #11551, #10686, .T. ) ;
#9204 = AXIS2_PLACEMENT_3D ( 'NONE', #8458, #231, #15598 ) ;
#9205 = DIRECTION ( 'NONE',  ( 0.000000000000000000, -1.000000000000000000, 0.000000000000000000 ) ) ;
#9206 = ORIENTED_EDGE ( 'NONE', *, *, #16809, .T. ) ;
#9207 = PRODUCT ( 'spur gear 1_iso_ISO - Spur gear 3M 40T 20PA 10FW ---S40A75H50L60.0N', 'spur gear 1_iso_ISO - Spur gear 3M 40T 20PA 10FW ---S40A75H50L60.0N', '', ( #130 ) ) ;
#9208 = ORIENTED_EDGE ( 'NONE', *, *, #18603, .F. ) ;
#9209 = PLANE ( 'NONE',  #11767 ) ;
#9210 = LINE ( 'NONE', #13984, #11093 ) ;
#9211 = CARTESIAN_POINT ( 'NONE',  ( 10.00000000000000000, -56.37237871411034718, 1.017308535512174261 ) ) ;
#9212 = ORIENTED_EDGE ( 'NONE', *, *, #7718, .F. ) ;
#9213 = DIRECTION ( 'NONE',  ( -0.000000000000000000, 1.000000000000000000, -0.000000000000000000 ) ) ;
#9214 = VECTOR ( 'NONE', #11088, 1000.000000000000000 ) ;
#9215 = DIRECTION ( 'NONE',  ( 1.000000000000000000, 0.000000000000000000, 0.000000000000000000 ) ) ;
#9216 = FACE_OUTER_BOUND ( 'NONE', #4893, .T. ) ;
#9217 = CARTESIAN_POINT ( 'NONE',  ( 11.14999999999999680, 0.000000000000000000, 30.00000000000000711 ) ) ;
#9218 = VERTEX_POINT ( 'NONE', #8016 ) ;
#9219 = CIRCLE ( 'NONE', #5267, 2.649999999999992806 ) ;
#9220 = CARTESIAN_POINT ( 'NONE',  ( 10.00000000000000000, 55.33199130079785277, 10.11537145609396404 ) ) ;
#9221 = EDGE_LOOP ( 'NONE', ( #16195, #9115, #18508, #238 ) ) ;
#9222 = CARTESIAN_POINT ( 'NONE',  ( 10.00000000000000000, 27.94286728106398243, -3.730438010304017116 ) ) ;
#9223 = CARTESIAN_POINT ( 'NONE',  ( -90.00000000009001155, -30.00000000000000000, -1.301042606982605321E-15 ) ) ;
#9224 = EDGE_CURVE ( 'NONE', #9000, #14712, #10327, .T. ) ;
#9225 = ADVANCED_FACE ( 'NONE', ( #9539 ), #902, .T. ) ;
#9226 = EDGE_CURVE ( 'NONE', #6022, #10989, #2112, .T. ) ;
#9227 = AXIS2_PLACEMENT_3D ( 'NONE', #4421, #8526, #10234 ) ;
#9228 = EDGE_CURVE ( 'NONE', #941, #5630, #4548, .T. ) ;
#9229 = B_SPLINE_CURVE_WITH_KNOTS ( 'NONE', 3,
 ( #11939, #4895, #1750, #7564, #6222, #17750, #6323, #4698 ),
 .UNSPECIFIED., .F., .F.,
 ( 4, 2, 2, 4 ),
 ( 7.780516681398759253E-20, 0.002450665683189819696, 0.003675998524784729327, 0.004901331366379639391 ),
 .UNSPECIFIED. ) ;
#9230 = VERTEX_POINT ( 'NONE', #6409 ) ;
#9231 = DIRECTION ( 'NONE',  ( 1.000000000000000000, 0.000000000000000000, 0.000000000000000000 ) ) ;
#9232 = ADVANCED_FACE ( 'NONE', ( #2301 ), #3832, .T. ) ;
#9233 = VERTEX_POINT ( 'NONE', #603 ) ;
#9234 = FACE_OUTER_BOUND ( 'NONE', #17725, .T. ) ;
#9235 = DIRECTION ( 'NONE',  ( -1.000000000000000000, -0.000000000000000000, -0.000000000000000000 ) ) ;
#9236 = EDGE_CURVE ( 'NONE', #5310, #16839, #13377, .T. ) ;
#9237 = DIRECTION ( 'NONE',  ( 0.000000000000000000, 1.000000000000000000, 0.000000000000000000 ) ) ;
#9238 = CARTESIAN_POINT ( 'NONE',  ( 10.04305231718605285, -26.50000000000000000, -30.90933677959240811 ) ) ;
#9239 = DIRECTION ( 'NONE',  ( 1.000000000000000000, -0.000000000000000000, -0.000000000000000000 ) ) ;
#9240 = ORIENTED_EDGE ( 'NONE', *, *, #14283, .T. ) ;
#9241 = CARTESIAN_POINT ( 'NONE',  ( 10.00000000000000000, 0.000000000000000000, 0.000000000000000000 ) ) ;
#9242 = MANIFOLD_SOLID_BREP ( 'Body', #17433 ) ;
#9243 = PRESENTATION_LAYER_ASSIGNMENT (  '', '', ( #10161 ) ) ;
#9244 = CARTESIAN_POINT ( 'NONE',  ( -4.198928548860774157, 0.8158838809860065044, -3.526471437616918170 ) ) ;
#9245 = ORIENTED_EDGE ( 'NONE', *, *, #8383, .F. ) ;
#9246 = EDGE_CURVE ( 'NONE', #16356, #1379, #6599, .T. ) ;
#9247 = ITEM_DEFINED_TRANSFORMATION ( 'NONE', 'NONE', #11993,  #8017 ) ;
#9248 = EDGE_LOOP ( 'NONE', ( #16711, #2100, #8641, #12134 ) ) ;
#9249 = ORIENTED_EDGE ( 'NONE', *, *, #4388, .T. ) ;
#9250 = EDGE_CURVE ( 'NONE', #10416, #17956, #12231, .T. ) ;
#9251 = EDGE_LOOP ( 'NONE', ( #17349, #9196 ) ) ;
#9252 = CARTESIAN_POINT ( 'NONE',  ( 0.000000000000000000, 0.000000000000000000, 0.000000000000000000 ) ) ;
#9253 = CARTESIAN_POINT ( 'NONE',  ( -10.00000000000000000, -26.45033635316118747, 36.40576474687271258 ) ) ;
#9254 = CIRCLE ( 'NONE', #1064, 12.00000000001200640 ) ;
#9255 = CARTESIAN_POINT ( 'NONE',  ( -5.032868406504333869, -28.36021363089093938, -2.000000000000000000 ) ) ;
#9256 = FACE_OUTER_BOUND ( 'NONE', #14855, .T. ) ;
#9257 = DIRECTION ( 'NONE',  ( -1.000000000000000000, -0.000000000000000000, -0.000000000000000000 ) ) ;
#9258 = FACE_BOUND ( 'NONE', #14884, .T. ) ;
#9259 = FACE_OUTER_BOUND ( 'NONE', #5020, .T. ) ;
#9260 = ORIENTED_EDGE ( 'NONE', *, *, #4123, .T. ) ;
#9261 = DIRECTION ( 'NONE',  ( 0.000000000000000000, -1.000000000000000000, 0.000000000000000000 ) ) ;
#9262 = ORIENTED_EDGE ( 'NONE', *, *, #16405, .T. ) ;
#9263 = CARTESIAN_POINT ( 'NONE',  ( 5.000000000000000000, -32.46095361140688595, -5.940243314904557259 ) ) ;
#9264 = FACE_OUTER_BOUND ( 'NONE', #13459, .T. ) ;
#9265 = DIRECTION ( 'NONE',  ( 0.000000000000000000, 0.000000000000000000, 1.000000000000000000 ) ) ;
#9266 = ORIENTED_EDGE ( 'NONE', *, *, #14347, .F. ) ;
#9267 = VERTEX_POINT ( 'NONE', #17954 ) ;
#9268 = DIRECTION ( 'NONE',  ( 0.000000000000000000, 0.000000000000000000, 1.000000000000000000 ) ) ;
#9269 = DIRECTION ( 'NONE',  ( 0.000000000000000000, 0.000000000000000000, 1.000000000000000000 ) ) ;
#9270 = PRESENTATION_LAYER_ASSIGNMENT (  '', '', ( #18083 ) ) ;
#9271 = CYLINDRICAL_SURFACE ( 'NONE', #18409, 63.00000000006298961 ) ;
#9272 = VERTEX_POINT ( 'NONE', #2230 ) ;
#9273 = VECTOR ( 'NONE', #10246, 1000.000000000000000 ) ;
#9274 = EDGE_CURVE ( 'NONE', #6354, #5152, #13955, .T. ) ;
#9275 = CARTESIAN_POINT ( 'NONE',  ( 10.00000000000000000, -42.79754323328189969, -13.90576474687263264 ) ) ;
#9276 = FACE_BOUND ( 'NONE', #9895, .T. ) ;
#9277 = FACE_OUTER_BOUND ( 'NONE', #5756, .T. ) ;
#9278 = ORIENTED_EDGE ( 'NONE', *, *, #6095, .T. ) ;
#9279 = DIRECTION ( 'NONE',  ( 0.000000000000000000, 0.000000000000000000, 1.000000000000000000 ) ) ;
#9280 = DIRECTION ( 'NONE',  ( 0.000000000000000000, 1.224646799147353207E-16, 1.000000000000000000 ) ) ;
#9281 = AXIS2_PLACEMENT_3D ( 'NONE', #13396, #9096, #343 ) ;
#9282 = ORIENTED_EDGE ( 'NONE', *, *, #7422, .T. ) ;
#9283 = CARTESIAN_POINT ( 'NONE',  ( 0.000000000000000000, 0.000000000000000000, 0.000000000000000000 ) ) ;
#9284 = CIRCLE ( 'NONE', #16900, 2.649999999999992806 ) ;
#9285 = ORIENTED_EDGE ( 'NONE', *, *, #5027, .F. ) ;
#9286 = CARTESIAN_POINT ( 'NONE',  ( 4.999999999999999112, 24.97244012287502102, 57.83923611457328207 ) ) ;
#9287 = CARTESIAN_POINT ( 'NONE',  ( 0.000000000000000000, -55.74967257055877212, -7.478235706489567924 ) ) ;
#9288 = ORIENTED_EDGE ( 'NONE', *, *, #4908, .T. ) ;
#9289 = ORIENTED_EDGE ( 'NONE', *, *, #12500, .F. ) ;
#9290 = LINE ( 'NONE', #6066, #18418 ) ;
#9291 = EDGE_CURVE ( 'NONE', #1567, #139, #8036, .T. ) ;
#9292 = VERTEX_POINT ( 'NONE', #920 ) ;
#9293 = CARTESIAN_POINT ( 'NONE',  ( 10.04305231718605285, -30.00000000000000000, -28.25933677959240953 ) ) ;
#9294 = AXIS2_PLACEMENT_3D ( 'NONE', #4894, #11143, #610 ) ;
#9295 = ADVANCED_FACE ( 'NONE', ( #4905 ), #13846, .T. ) ;
#9296 = AXIS2_PLACEMENT_3D ( 'NONE', #16499, #9161, #7727 ) ;
#9297 = CIRCLE ( 'NONE', #1686, 2.500000000000000888 ) ;
#9298 = CARTESIAN_POINT ( 'NONE',  ( 4.175648173966055587, -2.207990556236547608, -3.469390959564065291 ) ) ;
#9299 = EDGE_LOOP ( 'NONE', ( #14363, #16893, #14652, #12217 ) ) ;
#9300 = ORIENTED_EDGE ( 'NONE', *, *, #2489, .F. ) ;
#9301 = CARTESIAN_POINT ( 'NONE',  ( 2.756197834950227410, 3.027510591568626896, -3.223146290109805356 ) ) ;
#9302 = DIRECTION ( 'NONE',  ( 0.000000000000000000, 1.000000000000000000, 0.000000000000000000 ) ) ;
#9304 = PRESENTATION_LAYER_ASSIGNMENT (  '', '', ( #3240 ) ) ;
#9303 = DIRECTION ( 'NONE',  ( -1.000000000000000000, 0.000000000000000000, -0.000000000000000000 ) ) ;
#9305 = VERTEX_POINT ( 'NONE', #6718 ) ;
#9306 = DIRECTION ( 'NONE',  ( 0.000000000000000000, 0.000000000000000000, 1.000000000000000000 ) ) ;
#9307 = CIRCLE ( 'NONE', #8092, 2.396904916527700102 ) ;
#9308 = CARTESIAN_POINT ( 'NONE',  ( 0.000000000000000000, 56.23315539212690339, -1.335003989221823062 ) ) ;
#9309 = CARTESIAN_POINT ( 'NONE',  ( 3.098410542199072637, -7.060458129626440815, 0.000000000000000000 ) ) ;
#9310 = AXIS2_PLACEMENT_3D ( 'NONE', #25, #14486, #9917 ) ;
#9311 = CARTESIAN_POINT ( 'NONE',  ( 4.999999999999999112, -54.20017844242534721, 32.11449294037177538 ) ) ;
#9312 = ORIENTED_EDGE ( 'NONE', *, *, #10736, .T. ) ;
#9313 = VECTOR ( 'NONE', #17966, 1000.000000000000000 ) ;
#9314 = DIRECTION ( 'NONE',  ( -1.000000000000000000, 0.000000000000000000, 0.000000000000000000 ) ) ;
#9315 = VERTEX_POINT ( 'NONE', #10897 ) ;
#9316 = DIRECTION ( 'NONE',  ( -1.000000000000000000, -0.000000000000000000, -0.000000000000000000 ) ) ;
#9317 = DIRECTION ( 'NONE',  ( 0.000000000000000000, 0.000000000000000000, -1.000000000000000000 ) ) ;
#9318 = AXIS2_PLACEMENT_3D ( 'NONE', #13721, #5139, #2277 ) ;
#9319 = AXIS2_PLACEMENT_3D ( 'NONE', #8082, #15235, #11316 ) ;
#9320 = CIRCLE ( 'NONE', #3559, 2.649999999999999467 ) ;
#9321 = CIRCLE ( 'NONE', #4465, 30.00000000000000000 ) ;
#9322 = ORIENTED_EDGE ( 'NONE', *, *, #686, .F. ) ;
#9323 = VERTEX_POINT ( 'NONE', #3482 ) ;
#9324 = DIRECTION ( 'NONE',  ( 0.000000000000000000, 0.5877852522924686962, 0.8090169943749507819 ) ) ;
#9325 = PLANE ( 'NONE',  #16639 ) ;
#9326 = LINE ( 'NONE', #12284, #1136 ) ;
#9327 = ADVANCED_FACE ( 'NONE', ( #4989 ), #13760, .F. ) ;
#9328 = ADVANCED_FACE ( 'NONE', ( #818, #18138, #2144, #9276, #6622, #15009, #3584, #5090, #9556, #7947, #10619, #6340, #15371 ), #3763, .F. ) ;
#9329 = DIRECTION ( 'NONE',  ( 0.000000000000000000, 0.000000000000000000, 1.000000000000000000 ) ) ;
#9330 = AXIS2_PLACEMENT_3D ( 'NONE', #3332, #14742, #363 ) ;
#9331 = CARTESIAN_POINT ( 'NONE',  ( -11.15000000000000391, 3.661693929450586610E-15, -29.90000000000000213 ) ) ;
#9332 = VERTEX_POINT ( 'NONE', #12428 ) ;
#9333 = DIRECTION ( 'NONE',  ( 0.1586811557617541224, 0.000000000000000000, 0.9873298794253690946 ) ) ;
#9334 = CIRCLE ( 'NONE', #2050, 12.00000000001200640 ) ;
#9335 = EDGE_CURVE ( 'NONE', #4356, #10680, #16123, .T. ) ;
#9336 = FACE_OUTER_BOUND ( 'NONE', #15866, .T. ) ;
#9337 = VERTEX_POINT ( 'NONE', #2326 ) ;
#9338 = VECTOR ( 'NONE', #13848, 1000.000000000000000 ) ;
#9339 = AXIS2_PLACEMENT_3D ( 'NONE', #5507, #11306, #3985 ) ;
#9340 = CONTEXT_DEPENDENT_SHAPE_REPRESENTATION ( #16203, #17421 ) ;
#9341 = EDGE_CURVE ( 'NONE', #10019, #9230, #7902, .T. ) ;
#9342 = ORIENTED_EDGE ( 'NONE', *, *, #141, .F. ) ;
#9343 = ORIENTED_EDGE ( 'NONE', *, *, #17857, .T. ) ;
#9344 = EDGE_CURVE ( 'NONE', #9531, #18077, #12174, .T. ) ;
#9345 = CIRCLE ( 'NONE', #864, 12.00000000001200284 ) ;
#9346 = ORIENTED_EDGE ( 'NONE', *, *, #12828, .F. ) ;
#9347 = CIRCLE ( 'NONE', #13625, 24.00000000002399858 ) ;
#9348 = LINE ( 'NONE', #16788, #14189 ) ;
#9349 = DIRECTION ( 'NONE',  ( -1.000000000000000000, -0.000000000000000000, 0.000000000000000000 ) ) ;
#9350 = CIRCLE ( 'NONE', #553, 24.00000000002399148 ) ;
#9351 = CIRCLE ( 'NONE', #4787, 0.7500000000000000000 ) ;
#9352 = DIRECTION ( 'NONE',  ( -1.000000000000000000, -0.000000000000000000, -0.000000000000000000 ) ) ;
#9353 = DIRECTION ( 'NONE',  ( 1.000000000000000000, 0.000000000000000000, 0.000000000000000000 ) ) ;
#9354 = EDGE_CURVE ( 'NONE', #7704, #15596, #626, .T. ) ;
#9355 = ADVANCED_FACE ( 'NONE', ( #18044 ), #3388, .F. ) ;
#9356 = CARTESIAN_POINT ( 'NONE',  ( -79.64793068852898728, -38.00000000000000000, -34.51039329588756033 ) ) ;
#9357 = DIRECTION ( 'NONE',  ( -0.000000000000000000, 1.000000000000000000, -0.000000000000000000 ) ) ;
#9358 = DIRECTION ( 'NONE',  ( 0.000000000000000000, 0.000000000000000000, -1.000000000000000000 ) ) ;
#9359 = ORIENTED_EDGE ( 'NONE', *, *, #3433, .F. ) ;
#9360 = CYLINDRICAL_SURFACE ( 'NONE', #11204, 6.080745460913608902 ) ;
#9361 = ORIENTED_EDGE ( 'NONE', *, *, #11326, .F. ) ;
#9362 = ADVANCED_FACE ( 'NONE', ( #13580 ), #10795, .T. ) ;
#9363 = CARTESIAN_POINT ( 'NONE',  ( 0.000000000000000000, 0.000000000000000000, 0.000000000000000000 ) ) ;
#9364 = CARTESIAN_POINT ( 'NONE',  ( -79.64793068852927149, -30.00000000000000000, 34.51039329588763138 ) ) ;
#9365 = CARTESIAN_POINT ( 'NONE',  ( 10.00000000000000000, 0.000000000000000000, 0.000000000000000000 ) ) ;
#9366 = VECTOR ( 'NONE', #6059, 1000.000000000000114 ) ;
#9367 = ORIENTED_EDGE ( 'NONE', *, *, #15278, .F. ) ;
#9368 = ORIENTED_EDGE ( 'NONE', *, *, #2154, .T. ) ;
#9369 = EDGE_CURVE ( 'NONE', #17227, #9008, #10045, .T. ) ;
#9370 = DIRECTION ( 'NONE',  ( 0.000000000000000000, -1.000000000000000000, -1.040834085585042960E-14 ) ) ;
#9371 = DIRECTION ( 'NONE',  ( 6.123233995736766036E-17, -1.000000000000000000, 0.000000000000000000 ) ) ;
#9372 = AXIS2_PLACEMENT_3D ( 'NONE', #11342, #1261, #5626 ) ;
#9373 = DIRECTION ( 'NONE',  ( -1.000000000000000000, -0.000000000000000000, -0.000000000000000000 ) ) ;
#9374 = ORIENTED_EDGE ( 'NONE', *, *, #15636, .F. ) ;
#9375 = CIRCLE ( 'NONE', #6023, 26.24900000002625333 ) ;
#9376 = AXIS2_PLACEMENT_3D ( 'NONE', #7809, #9237, #16399 ) ;
#9377 = PRODUCT ( 'stationary ring', 'stationary ring', '', ( #18698 ) ) ;
#9378 = DIRECTION ( 'NONE',  ( 0.000000000000000000, 0.000000000000000000, 1.000000000000000000 ) ) ;
#9379 = CARTESIAN_POINT ( 'NONE',  ( 10.00000000000000000, 32.31183295104772668, 46.20417134726143615 ) ) ;
#9380 = AXIS2_PLACEMENT_3D ( 'NONE', #11376, #8521, #1294 ) ;
#9381 = DIRECTION ( 'NONE',  ( 0.000000000000000000, 0.000000000000000000, 1.000000000000000000 ) ) ;
#9382 = VERTEX_POINT ( 'NONE', #5278 ) ;
#9383 = DIRECTION ( 'NONE',  ( -1.000000000000000000, 0.000000000000000000, 0.000000000000000000 ) ) ;
#9384 = VECTOR ( 'NONE', #4386, 1000.000000000000000 ) ;
#9385 = PRESENTATION_LAYER_ASSIGNMENT (  '', '', ( #6361 ) ) ;
#9386 = ORIENTED_EDGE ( 'NONE', *, *, #11285, .T. ) ;
#9387 = AXIS2_PLACEMENT_3D ( 'NONE', #15603, #6462, #16073 ) ;
#9388 = CARTESIAN_POINT ( 'NONE',  ( -90.00000000009001155, 2.000000000000001776, -1.301042606982603940E-15 ) ) ;
#9389 = VERTEX_POINT ( 'NONE', #17296 ) ;
#9390 =( REPRESENTATION_RELATIONSHIP ('NONE','NONE', #11014, #2517 ) REPRESENTATION_RELATIONSHIP_WITH_TRANSFORMATION ( #2397 )SHAPE_REPRESENTATION_RELATIONSHIP( ) );
#9391 = CARTESIAN_POINT ( 'NONE',  ( 0.000000000000000000, -49.76630880786289879, -26.49895292618059273 ) ) ;
#9392 = DIRECTION ( 'NONE',  ( -1.000000000000000000, -0.000000000000000000, -0.000000000000000000 ) ) ;
#9393 = ORIENTED_EDGE ( 'NONE', *, *, #11950, .T. ) ;
#9394 = ORIENTED_EDGE ( 'NONE', *, *, #1042, .F. ) ;
#9395 = EDGE_CURVE ( 'NONE', #91, #14712, #10341, .T. ) ;
#9396 = CARTESIAN_POINT ( 'NONE',  ( 45.00000000000000000, 10.00000000000000000, -5.120903701083534543E-13 ) ) ;
#9397 = FILL_AREA_STYLE_COLOUR ( '', #18065 ) ;
#9398 = ORIENTED_EDGE ( 'NONE', *, *, #18415, .T. ) ;
#9399 = DIRECTION ( 'NONE',  ( 0.000000000000000000, 0.000000000000000000, -1.000000000000000000 ) ) ;
#9400 = VECTOR ( 'NONE', #2987, 1000.000000000000000 ) ;
#9401 = CARTESIAN_POINT ( 'NONE',  ( 0.000000000000000000, 0.000000000000000000, 0.000000000000000000 ) ) ;
#9402 = DIRECTION ( 'NONE',  ( 0.000000000000000000, 0.000000000000000000, 1.000000000000000000 ) ) ;
#9403 = ORIENTED_EDGE ( 'NONE', *, *, #18434, .F. ) ;
#9404 = EDGE_CURVE ( 'NONE', #16644, #11649, #1289, .T. ) ;
#9405 = VECTOR ( 'NONE', #11811, 1000.000000000000114 ) ;
#9406 = VERTEX_POINT ( 'NONE', #12811 ) ;
#9407 = DIRECTION ( 'NONE',  ( 1.224646799147353207E-16, 1.000000000000000000, 0.000000000000000000 ) ) ;
#9408 = CARTESIAN_POINT ( 'NONE',  ( 0.000000000000000000, 1.489278925039520640, 26.20671763660629239 ) ) ;
#9409 = CARTESIAN_POINT ( 'NONE',  ( 2.500000000000000000, 0.000000000000000000, 0.000000000000000000 ) ) ;
#9410 = EDGE_LOOP ( 'NONE', ( #18457, #14770, #6298, #8508 ) ) ;
#9411 = DIRECTION ( 'NONE',  ( 0.000000000000000000, 0.000000000000000000, -1.000000000000000000 ) ) ;
#9412 = EDGE_CURVE ( 'NONE', #5044, #5875, #16435, .T. ) ;
#9413 = DIRECTION ( 'NONE',  ( -1.000000000000000000, -0.000000000000000000, 0.000000000000000000 ) ) ;
#9414 = FACE_BOUND ( 'NONE', #7166, .T. ) ;
#9415 = CARTESIAN_POINT ( 'NONE',  ( -1.828356344711647319, -3.563200125723192002, -1.076197711133951296E-14 ) ) ;
#9416 = ORIENTED_EDGE ( 'NONE', *, *, #10927, .T. ) ;
#9417 = FACE_OUTER_BOUND ( 'NONE', #18141, .T. ) ;
#9418 = ORIENTED_EDGE ( 'NONE', *, *, #12852, .F. ) ;
#9419 = DIRECTION ( 'NONE',  ( -1.000000000000000000, -0.000000000000000000, -0.000000000000000000 ) ) ;
#9420 = DIRECTION ( 'NONE',  ( -1.000000000000000000, 0.000000000000000000, 0.000000000000000000 ) ) ;
#9421 = AXIS2_PLACEMENT_3D ( 'NONE', #4337, #11486, #14425 ) ;
#9422 = AXIS2_PLACEMENT_3D ( 'NONE', #11656, #4327, #14784 ) ;
#9423 = EDGE_CURVE ( 'NONE', #11781, #9323, #9464, .T. ) ;
#9424 = ORIENTED_EDGE ( 'NONE', *, *, #562, .F. ) ;
#9425 = ORIENTED_EDGE ( 'NONE', *, *, #8616, .F. ) ;
#9426 = CARTESIAN_POINT ( 'NONE',  ( 32.50000000000000000, -26.50000000000000000, 3.680389326632394941E-13 ) ) ;
#9427 = DIRECTION ( 'NONE',  ( 0.000000000000000000, 0.000000000000000000, 1.000000000000000000 ) ) ;
#9428 = DIRECTION ( 'NONE',  ( -1.000000000000000000, 0.000000000000000000, 0.000000000000000000 ) ) ;
#9429 = CARTESIAN_POINT ( 'NONE',  ( -90.00000000009001155, 1.000000000000014655, -1.301042606982603940E-15 ) ) ;
#9430 = EDGE_CURVE ( 'NONE', #8692, #15353, #2430, .T. ) ;
#9431 = DIRECTION ( 'NONE',  ( -1.000000000000000000, 0.000000000000000000, 0.000000000000000000 ) ) ;
#9432 = LINE ( 'NONE', #7712, #17212 ) ;
#9433 = VERTEX_POINT ( 'NONE', #8518 ) ;
#9435 = DIRECTION ( 'NONE',  ( -1.000000000000000000, -0.000000000000000000, 0.000000000000000000 ) ) ;
#9434 = AXIS2_PLACEMENT_3D ( 'NONE', #3175, #17563, #3089 ) ;
#9436 = VECTOR ( 'NONE', #4218, 1000.000000000000000 ) ;
#9437 = FILL_AREA_STYLE ('',( #398 ) ) ;
#9438 = LINE ( 'NONE', #7815, #13632 ) ;
#9439 = VERTEX_POINT ( 'NONE', #14417 ) ;
#9440 = CONTEXT_DEPENDENT_SHAPE_REPRESENTATION ( #18146, #4812 ) ;
#9441 = ORIENTED_EDGE ( 'NONE', *, *, #9947, .T. ) ;
#9442 = EDGE_CURVE ( 'NONE', #9803, #4207, #14000, .T. ) ;
#9443 = EDGE_CURVE ( 'NONE', #298, #17641, #4145, .T. ) ;
#9444 = ORIENTED_EDGE ( 'NONE', *, *, #3407, .T. ) ;
#9445 = ORIENTED_EDGE ( 'NONE', *, *, #18667, .F. ) ;
#9446 = DIRECTION ( 'NONE',  ( -1.000000000000000000, 0.000000000000000000, -0.000000000000000000 ) ) ;
#9447 = DIRECTION ( 'NONE',  ( -1.000000000000000000, -0.000000000000000000, -0.000000000000000000 ) ) ;
#9448 = PRESENTATION_STYLE_ASSIGNMENT (( #15346 ) ) ;
#9449 = DIRECTION ( 'NONE',  ( 0.000000000000000000, 0.000000000000000000, -1.000000000000000000 ) ) ;
#9450 =( NAMED_UNIT ( * ) SI_UNIT ( $, .STERADIAN. ) SOLID_ANGLE_UNIT ( ) );
#9451 = CARTESIAN_POINT ( 'NONE',  ( 2.500000000000000000, 2.357898499370432166, -2.385244779468109755E-15 ) ) ;
#9452 = CARTESIAN_POINT ( 'NONE',  ( 10.00000000000000000, -7.478235706489372525, 55.74967257055880054 ) ) ;
#9453 = DIRECTION ( 'NONE',  ( 0.000000000000000000, 0.000000000000000000, 1.000000000000000000 ) ) ;
#9454 = ORIENTED_EDGE ( 'NONE', *, *, #18443, .T. ) ;
#9455 = DIRECTION ( 'NONE',  ( -1.000000000000000000, 0.000000000000000000, -0.000000000000000000 ) ) ;
#9456 = ORIENTED_EDGE ( 'NONE', *, *, #10220, .F. ) ;
#9457 = EDGE_CURVE ( 'NONE', #923, #11328, #7307, .T. ) ;
#9458 = CARTESIAN_POINT ( 'NONE',  ( 0.1481481481481481122, -4.797713218419819903, -1.000000000000000000 ) ) ;
#9459 = LINE ( 'NONE', #18402, #4783 ) ;
#9460 = VERTEX_POINT ( 'NONE', #3858 ) ;
#9461 = ORIENTED_EDGE ( 'NONE', *, *, #5088, .T. ) ;
#9462 = CARTESIAN_POINT ( 'NONE',  ( -2.682243648011671588, -3.070208061305317759, -0.04852650426602272971 ) ) ;
#9463 = AXIS2_PLACEMENT_3D ( 'NONE', #17866, #17763, #5953 ) ;
#9464 = B_SPLINE_CURVE_WITH_KNOTS ( 'NONE', 3,
 ( #15571, #7084, #6899, #15480, #5660, #5484 ),
 .UNSPECIFIED., .F., .F.,
 ( 4, 2, 4 ),
 ( 0.002452478801916361129, 0.003676905084148001344, 0.004901331366379641126 ),
 .UNSPECIFIED. ) ;
#9465 = CARTESIAN_POINT ( 'NONE',  ( -26.29305231718584324, -34.99999999999999289, 19.10302069950530779 ) ) ;
#9466 = ORIENTED_EDGE ( 'NONE', *, *, #5525, .T. ) ;
#9467 = ADVANCED_FACE ( 'NONE', ( #11078 ), #12715, .F. ) ;
#9468 = EDGE_CURVE ( 'NONE', #2107, #17109, #9742, .T. ) ;
#9469 = ADVANCED_FACE ( 'NONE', ( #18705 ), #11476, .T. ) ;
#9470 = DIRECTION ( 'NONE',  ( -0.000000000000000000, 1.000000000000000000, -0.000000000000000000 ) ) ;
#9471 = EDGE_CURVE ( 'NONE', #4068, #12311, #12522, .T. ) ;
#9472 = DIRECTION ( 'NONE',  ( -0.000000000000000000, 1.000000000000000000, -0.000000000000000000 ) ) ;
#9473 = CARTESIAN_POINT ( 'NONE',  ( 0.000000000000000000, 24.79895094899259789, -13.40641754777674421 ) ) ;
#9474 = VERTEX_POINT ( 'NONE', #17013 ) ;
#9476 = LINE ( 'NONE', #13958, #11288 ) ;
#9475 = AXIS2_PLACEMENT_3D ( 'NONE', #8700, #13376, #4515 ) ;
#9477 = VERTEX_POINT ( 'NONE', #3963 ) ;
#9478 = DIRECTION ( 'NONE',  ( -1.000000000000000000, 0.000000000000000000, 0.000000000000000000 ) ) ;
#9479 = ORIENTED_EDGE ( 'NONE', *, *, #5167, .T. ) ;
#9480 = EDGE_CURVE ( 'NONE', #10707, #1691, #9761, .T. ) ;
#9481 = CIRCLE ( 'NONE', #3104, 29.90000000000000213 ) ;
#9482 = CARTESIAN_POINT ( 'NONE',  ( -11.25000000000000355, 0.000000000000000000, 0.000000000000000000 ) ) ;
#9483 = CIRCLE ( 'NONE', #18011, 24.00000000002399503 ) ;
#9484 = LINE ( 'NONE', #5100, #9214 ) ;
#9485 = DIRECTION ( 'NONE',  ( 1.000000000000000000, 0.000000000000000000, 0.000000000000000000 ) ) ;
#9486 = ORIENTED_EDGE ( 'NONE', *, *, #15721, .T. ) ;
#9487 = ORIENTED_EDGE ( 'NONE', *, *, #5167, .F. ) ;
#9488 = CARTESIAN_POINT ( 'NONE',  ( -10.00000000000000000, 26.45033635316149301, 39.05576474687247668 ) ) ;
#9489 = ORIENTED_EDGE ( 'NONE', *, *, #10036, .T. ) ;
#9490 = CARTESIAN_POINT ( 'NONE',  ( -12.69999999999999929, 0.000000000000000000, 0.000000000000000000 ) ) ;
#9491 = EDGE_CURVE ( 'NONE', #3305, #684, #12163, .T. ) ;
#9492 = AXIS2_PLACEMENT_3D ( 'NONE', #1660, #16151, #9092 ) ;
#9493 = CARTESIAN_POINT ( 'NONE',  ( 0.000000000000000000, 0.000000000000000000, 0.000000000000000000 ) ) ;
#9494 = LINE ( 'NONE', #18546, #11163 ) ;
#9495 = ADVANCED_FACE ( 'NONE', ( #2611 ), #7001, .F. ) ;
#9496 = VERTEX_POINT ( 'NONE', #11575 ) ;
#9497 = ORIENTED_EDGE ( 'NONE', *, *, #7196, .T. ) ;
#9498 = DIRECTION ( 'NONE',  ( -0.000000000000000000, 1.000000000000000000, -0.000000000000000000 ) ) ;
#9499 = DIRECTION ( 'NONE',  ( -1.000000000000000000, 0.000000000000000000, 0.000000000000000000 ) ) ;
#9500 = DIRECTION ( 'NONE',  ( -1.000000000000000000, 0.000000000000000000, 0.000000000000000000 ) ) ;
#9501 = ORIENTED_EDGE ( 'NONE', *, *, #16738, .F. ) ;
#9502 = FACE_OUTER_BOUND ( 'NONE', #18204, .T. ) ;
#9503 = EDGE_LOOP ( 'NONE', ( #1860, #17696, #6357, #7736 ) ) ;
#9504 = CARTESIAN_POINT ( 'NONE',  ( 0.000000000000000000, 0.000000000000000000, -2.000000000000000000 ) ) ;
#9505 = FACE_BOUND ( 'NONE', #8828, .T. ) ;
#9506 = ORIENTED_EDGE ( 'NONE', *, *, #4911, .F. ) ;
#9507 = EDGE_LOOP ( 'NONE', ( #17269, #3358, #4670, #14890 ) ) ;
#9508 = CARTESIAN_POINT ( 'NONE',  ( 10.00000000000000000, -53.29895248911688554, 18.38754094778222026 ) ) ;
#9509 = AXIS2_PLACEMENT_3D ( 'NONE', #12080, #15232, #368 ) ;
#9510 = ORIENTED_EDGE ( 'NONE', *, *, #2166, .F. ) ;
#9511 = CYLINDRICAL_SURFACE ( 'NONE', #13959, 12.00000000001200462 ) ;
#9512 = CIRCLE ( 'NONE', #7384, 24.00000000002400213 ) ;
#9513 = CARTESIAN_POINT ( 'NONE',  ( 10.00000000000000000, 0.000000000000000000, 0.000000000000000000 ) ) ;
#9514 = AXIS2_PLACEMENT_3D ( 'NONE', #11047, #16870, #9624 ) ;
#9515 = EDGE_CURVE ( 'NONE', #8709, #4490, #11572, .T. ) ;
#9516 = ORIENTED_EDGE ( 'NONE', *, *, #3913, .F. ) ;
#9517 = ORIENTED_EDGE ( 'NONE', *, *, #740, .T. ) ;
#9518 = CYLINDRICAL_SURFACE ( 'NONE', #18449, 25.00000000000000000 ) ;
#9519 = CLOSED_SHELL ( 'NONE', ( #5978, #15376, #13782, #2139, #7969, #5952, #500, #13771, #4255, #13736, #2937, #129, #4940, #15659, #7716, #17789, #866, #1899, #10486, #3413, #13777, #4514, #16582, #10640, #9225, #17835, #13193, #4531, #3361, #3647, #17721, #17460, #3176, #14484, #2446, #15643, #5808, #170, #6160, #18066, #723, #15304, #16194, #15135, #1047, #13571, #18135, #14271, #18086, #13904, #4620, #11452, #9017, #8317, #4359, #10864, #9566, #4195, #515, #11321, #11081, #15006, #10626, #16452, #8648, #3718, #4935, #16112, #7039, #730, #5144, #11076, #1054, #3432, #11033, #13902, #8786, #5453, #7903, #871, #2967, #9817, #15520, #12662, #4719, #6105, #2936, #269, #15099, #2114, #3335, #17524, #17772, #2000, #6663, #12018, #12815, #13215, #7835, #6681, #6802, #2779, #15210, #9106, #18257, #3167, #9830, #6576, #17628, #17924, #4683, #5648, #3411, #18519, #13371, #2793, #2798, #2729, #17995, #623, #17647, #6499, #16239, #18179, #3851, #12152, #16941, #8857, #3201, #4477, #17580, #12010, #4012, #8854, #18721, #2129, #9956, #9823, #9232, #10726, #18112, #7444, #7824, #16564, #3928, #18655, #8981, #17439, #12146, #14309, #15832, #1655, #13873, #9469, #16467, #9123, #10307, #1962, #18660, #18093, #7554, #12165, #17720, #10724, #9979, #324, #18785, #9362, #10225, #10411, #17165, #4928, #6449, #15936, #1502, #15177, #16944, #15642, #8534 ) ) ;
#9520 = CARTESIAN_POINT ( 'NONE',  ( 32.50000000000000000, -26.50000000000000000, 2.650000000000367617 ) ) ;
#9521 = DIRECTION ( 'NONE',  ( -0.000000000000000000, 1.000000000000000000, -0.000000000000000000 ) ) ;
#9522 = DIRECTION ( 'NONE',  ( 0.000000000000000000, -0.3090169943749547787, 0.9510565162951511997 ) ) ;
#9523 = LINE ( 'NONE', #2282, #12729 ) ;
#9524 = CARTESIAN_POINT ( 'NONE',  ( 10.00000000000000000, 0.000000000000000000, 0.000000000000000000 ) ) ;
#9525 = EDGE_LOOP ( 'NONE', ( #40, #6444, #8111, #7372 ) ) ;
#9526 = CARTESIAN_POINT ( 'NONE',  ( 0.000000000000000000, 0.000000000000000000, 0.000000000000000000 ) ) ;
#9527 = LINE ( 'NONE', #10762, #1470 ) ;
#9528 = VERTEX_POINT ( 'NONE', #3087 ) ;
#9529 = ADVANCED_FACE ( 'NONE', ( #133 ), #15941, .T. ) ;
#9530 = AXIS2_PLACEMENT_3D ( 'NONE', #11852, #7649, #3570 ) ;
#9531 = VERTEX_POINT ( 'NONE', #13000 ) ;
#9532 = ADVANCED_FACE ( 'NONE', ( #8965 ), #1560, .T. ) ;
#9533 = ORIENTED_EDGE ( 'NONE', *, *, #16153, .T. ) ;
#9534 = ORIENTED_EDGE ( 'NONE', *, *, #15401, .T. ) ;
#9535 = LINE ( 'NONE', #16591, #9014 ) ;
#9536 = CARTESIAN_POINT ( 'NONE',  ( 0.000000000000000000, -6.681932690257145424, 25.38428207620320265 ) ) ;
#9537 = DIRECTION ( 'NONE',  ( -1.000000000000000000, 0.000000000000000000, 0.000000000000000000 ) ) ;
#9538 = DIRECTION ( 'NONE',  ( -1.000000000000000000, -0.000000000000000000, -0.000000000000000000 ) ) ;
#9539 = FACE_OUTER_BOUND ( 'NONE', #12457, .T. ) ;
#9540 = AXIS2_PLACEMENT_3D ( 'NONE', #4320, #15932, #14227 ) ;
#9541 = DIRECTION ( 'NONE',  ( 0.000000000000000000, -0.8090169943749402348, -0.5877852522924830181 ) ) ;
#9542 = CARTESIAN_POINT ( 'NONE',  ( -36.40576474687247099, 10.00000000000000000, 23.80033635316149443 ) ) ;
#9543 = LINE ( 'NONE', #10971, #2588 ) ;
#9544 = ORIENTED_EDGE ( 'NONE', *, *, #12189, .F. ) ;
#9545 = DIRECTION ( 'NONE',  ( -1.000000000000000000, 0.000000000000000000, 0.000000000000000000 ) ) ;
#9546 = ORIENTED_EDGE ( 'NONE', *, *, #12793, .F. ) ;
#9547 = DIRECTION ( 'NONE',  ( 0.000000000000000000, 0.000000000000000000, -1.000000000000000000 ) ) ;
#9548 = DIRECTION ( 'NONE',  ( 0.000000000000000000, 0.000000000000000000, 1.000000000000000000 ) ) ;
#9549 = EDGE_LOOP ( 'NONE', ( #3568, #15386, #5519, #15136 ) ) ;
#9550 = ORIENTED_EDGE ( 'NONE', *, *, #16572, .F. ) ;
#9551 = DIRECTION ( 'NONE',  ( 0.000000000000000000, 0.000000000000000000, 1.000000000000000000 ) ) ;
#9552 = DIRECTION ( 'NONE',  ( -0.9052919020287826246, 7.285838599102589797E-17, -0.4247900329823064425 ) ) ;
#9553 = DIRECTION ( 'NONE',  ( -0.000000000000000000, -1.000000000000000000, -0.000000000000000000 ) ) ;
#9554 = ORIENTED_EDGE ( 'NONE', *, *, #9412, .T. ) ;
#9555 = CARTESIAN_POINT ( 'NONE',  ( -90.72413394419160682, -10.00000000000001599, 4.947285117213267469 ) ) ;
#9556 = FACE_BOUND ( 'NONE', #10099, .T. ) ;
#9557 = DIRECTION ( 'NONE',  ( 0.000000000000000000, 0.000000000000000000, 1.000000000000000000 ) ) ;
#9558 = ORIENTED_EDGE ( 'NONE', *, *, #13123, .T. ) ;
#9559 = CARTESIAN_POINT ( 'NONE',  ( -90.00000000009001155, -88.00000000000000000, -1.301042606982603940E-15 ) ) ;
#9560 = ORIENTED_EDGE ( 'NONE', *, *, #8065, .F. ) ;
#9561 = DIRECTION ( 'NONE',  ( -1.000000000000000000, -0.000000000000000000, -0.000000000000000000 ) ) ;
#9562 = EDGE_LOOP ( 'NONE', ( #9266, #16820, #3644, #3899 ) ) ;
#9563 = EDGE_CURVE ( 'NONE', #7010, #1366, #8516, .T. ) ;
#9564 = EDGE_CURVE ( 'NONE', #16736, #9315, #4554, .T. ) ;
#9565 = AXIS2_PLACEMENT_3D ( 'NONE', #14805, #4901, #1943 ) ;
#9566 = ADVANCED_FACE ( 'NONE', ( #2998 ), #16311, .T. ) ;
#9567 = CARTESIAN_POINT ( 'NONE',  ( 1.734723475976807094E-15, 4.618802153517012954, -0.4999999999999995559 ) ) ;
#9568 = DIRECTION ( 'NONE',  ( 1.000000000000000000, 0.000000000000000000, 0.000000000000000000 ) ) ;
#9569 = CARTESIAN_POINT ( 'NONE',  ( -117.1020693116508085, -30.00000000000000000, 19.69080595179778115 ) ) ;
#9570 = ORIENTED_EDGE ( 'NONE', *, *, #1792, .T. ) ;
#9571 = CIRCLE ( 'NONE', #13266, 63.00000000006298961 ) ;
#9572 = VERTEX_POINT ( 'NONE', #3270 ) ;
#9573 = VECTOR ( 'NONE', #16088, 1000.000000000000000 ) ;
#9574 = FACE_OUTER_BOUND ( 'NONE', #16630, .T. ) ;
#9575 = EDGE_CURVE ( 'NONE', #2531, #10475, #1233, .T. ) ;
#9576 = VERTEX_POINT ( 'NONE', #17464 ) ;
#9577 = CARTESIAN_POINT ( 'NONE',  ( 0.000000000000000000, 4.007856633824268044, -62.87238730325617553 ) ) ;
#9578 = EDGE_CURVE ( 'NONE', #5984, #1496, #10941, .T. ) ;
#9579 = CIRCLE ( 'NONE', #3320, 2.649999999999992806 ) ;
#9580 = CARTESIAN_POINT ( 'NONE',  ( 0.000000000000000000, 0.000000000000000000, 0.000000000000000000 ) ) ;
#9581 = EDGE_CURVE ( 'NONE', #8760, #5879, #4601, .T. ) ;
#9582 = CIRCLE ( 'NONE', #1672, 12.00000000001200640 ) ;
#9583 = DIRECTION ( 'NONE',  ( -0.000000000000000000, 1.000000000000000000, -0.000000000000000000 ) ) ;
#9584 = ORIENTED_EDGE ( 'NONE', *, *, #2841, .F. ) ;
#9585 = FILL_AREA_STYLE ('',( #15402 ) ) ;
#9586 = ORIENTED_EDGE ( 'NONE', *, *, #4405, .T. ) ;
#9587 = DIRECTION ( 'NONE',  ( -0.000000000000000000, -1.000000000000000000, -0.000000000000000000 ) ) ;
#9588 = DIRECTION ( 'NONE',  ( 0.000000000000000000, 0.000000000000000000, 1.000000000000000000 ) ) ;
#9589 = FACE_OUTER_BOUND ( 'NONE', #10562, .T. ) ;
#9590 = ORIENTED_EDGE ( 'NONE', *, *, #12732, .F. ) ;
#9591 = LINE ( 'NONE', #3792, #16955 ) ;
#9593 = VERTEX_POINT ( 'NONE', #8881 ) ;
#9592 = EDGE_CURVE ( 'NONE', #104, #2993, #16964, .T. ) ;
#9594 = EDGE_CURVE ( 'NONE', #7040, #12093, #13179, .T. ) ;
#9595 = LINE ( 'NONE', #12465, #16696 ) ;
#9596 = CARTESIAN_POINT ( 'NONE',  ( 0.000000000000000000, 0.000000000000000000, -1.000000000000000000 ) ) ;
#9597 = AXIS2_PLACEMENT_3D ( 'NONE', #8054, #13861, #836 ) ;
#9598 = ORIENTED_EDGE ( 'NONE', *, *, #4131, .F. ) ;
#9599 = ORIENTED_EDGE ( 'NONE', *, *, #2507, .F. ) ;
#9600 = ORIENTED_EDGE ( 'NONE', *, *, #9711, .F. ) ;
#9601 = CARTESIAN_POINT ( 'NONE',  ( 0.000000000000000000, 0.000000000000000000, 0.000000000000000000 ) ) ;
#9602 = DIRECTION ( 'NONE',  ( 0.000000000000000000, 0.000000000000000000, 1.000000000000000000 ) ) ;
#9603 = AXIS2_PLACEMENT_3D ( 'NONE', #16154, #12041, #625 ) ;
#9604 = AXIS2_PLACEMENT_3D ( 'NONE', #9054, #6196, #11997 ) ;
#9605 = ADVANCED_FACE ( 'NONE', ( #4512 ), #10323, .T. ) ;
#9606 = VECTOR ( 'NONE', #12138, 1000.000000000000000 ) ;
#9607 = PRESENTATION_LAYER_ASSIGNMENT (  '', '', ( #3839 ) ) ;
#9608 = ORIENTED_EDGE ( 'NONE', *, *, #1170, .T. ) ;
#9609 = VECTOR ( 'NONE', #11828, 1000.000000000000000 ) ;
#9610 = AXIS2_PLACEMENT_3D ( 'NONE', #1288, #7170, #14240 ) ;
#9611 = ORIENTED_EDGE ( 'NONE', *, *, #9404, .F. ) ;
#9612 = CARTESIAN_POINT ( 'NONE',  ( 10.00000000000000000, 49.49802920186260735, -26.71881558261677370 ) ) ;
#9613 = AXIS2_PLACEMENT_3D ( 'NONE', #9004, #351, #5960 ) ;
#9614 = CARTESIAN_POINT ( 'NONE',  ( 4.000000000000000000, 0.000000000000000000, 0.000000000000000000 ) ) ;
#9615 = CIRCLE ( 'NONE', #7141, 25.10000000000000142 ) ;
#9616 = DIRECTION ( 'NONE',  ( 0.000000000000000000, 0.000000000000000000, 1.000000000000000000 ) ) ;
#9617 = CARTESIAN_POINT ( 'NONE',  ( 0.000000000000000000, 0.000000000000000000, 0.000000000000000000 ) ) ;
#9618 = CARTESIAN_POINT ( 'NONE',  ( 4.999999999999999112, -5.940243314903991489, -32.46095361140699254 ) ) ;
#9619 = DIRECTION ( 'NONE',  ( -0.000000000000000000, -1.000000000000000000, -0.000000000000000000 ) ) ;
#9620 = DIRECTION ( 'NONE',  ( 1.000000000000000000, 0.000000000000000000, 0.000000000000000000 ) ) ;
#9621 = EDGE_LOOP ( 'NONE', ( #9155, #4029 ) ) ;
#9622 = DIRECTION ( 'NONE',  ( 0.000000000000000000, -0.4539904997395351471, -0.8910065241883737830 ) ) ;
#9623 = CYLINDRICAL_SURFACE ( 'NONE', #11813, 12.00000000001200462 ) ;
#9624 = DIRECTION ( 'NONE',  ( 0.000000000000000000, 0.000000000000000000, 1.000000000000000000 ) ) ;
#9625 = AXIS2_PLACEMENT_3D ( 'NONE', #1087, #18516, #5477 ) ;
#9626 = CIRCLE ( 'NONE', #12058, 63.00000000006298961 ) ;
#9627 = EDGE_CURVE ( 'NONE', #1507, #6567, #16136, .T. ) ;
#9628 = ITEM_DEFINED_TRANSFORMATION ( 'NONE', 'NONE', #17485,  #8017 ) ;
#9629 = AXIS2_PLACEMENT_3D ( 'NONE', #18094, #14965, #9145 ) ;
#9630 = VERTEX_POINT ( 'NONE', #4689 ) ;
#9631 = CIRCLE ( 'NONE', #12359, 12.00000000001200284 ) ;
#9632 = CIRCLE ( 'NONE', #3860, 28.00000000000000355 ) ;
#9633 = ORIENTED_EDGE ( 'NONE', *, *, #17508, .T. ) ;
#9634 = EDGE_LOOP ( 'NONE', ( #14943, #16876 ) ) ;
#9635 = CARTESIAN_POINT ( 'NONE',  ( -26.29305231718584324, -26.50000000000000000, 16.45302069950530566 ) ) ;
#9636 = CIRCLE ( 'NONE', #16335, 1.250000000000001110 ) ;
#9637 = DIRECTION ( 'NONE',  ( 0.000000000000000000, 0.000000000000000000, -1.000000000000000000 ) ) ;
#9638 = CARTESIAN_POINT ( 'NONE',  ( 10.00000000000000000, -5.120903701083534543E-13, -45.00000000000000000 ) ) ;
#9640 = DIRECTION ( 'NONE',  ( -1.000000000000000000, -0.000000000000000000, -0.000000000000000000 ) ) ;
#9639 = AXIS2_PLACEMENT_3D ( 'NONE', #5122, #13790, #16269 ) ;
#9641 = EDGE_CURVE ( 'NONE', #12447, #8465, #10058, .T. ) ;
#9642 = DIRECTION ( 'NONE',  ( -1.000000000000000000, -0.000000000000000000, 0.000000000000000000 ) ) ;
#9643 = DIRECTION ( 'NONE',  ( 0.000000000000000000, 0.000000000000000000, -1.000000000000000000 ) ) ;
#9644 = AXIS2_PLACEMENT_3D ( 'NONE', #13159, #7972, #14868 ) ;
#9645 = DIRECTION ( 'NONE',  ( 0.000000000000000000, 0.000000000000000000, 1.000000000000000000 ) ) ;
#9646 = ORIENTED_EDGE ( 'NONE', *, *, #12611, .T. ) ;
#9647 = VECTOR ( 'NONE', #4604, 1000.000000000000000 ) ;
#9648 = DIRECTION ( 'NONE',  ( -1.000000000000000000, 0.000000000000000000, 0.000000000000000000 ) ) ;
#9649 = ORIENTED_EDGE ( 'NONE', *, *, #578, .F. ) ;
#9650 = EDGE_CURVE ( 'NONE', #16064, #6648, #14923, .T. ) ;
#9651 = DIRECTION ( 'NONE',  ( 0.000000000000000000, 0.000000000000000000, 1.000000000000000000 ) ) ;
#9652 = CARTESIAN_POINT ( 'NONE',  ( -56.50000000009000445, -38.00000000000000000, 2.650000000000374278 ) ) ;
#9653 = EDGE_LOOP ( 'NONE', ( #16296, #5266, #14630, #11870 ) ) ;
#9654 = ORIENTED_EDGE ( 'NONE', *, *, #815, .F. ) ;
#9655 = DIRECTION ( 'NONE',  ( 1.000000000000000000, 0.000000000000000000, 0.000000000000000000 ) ) ;
#9656 = DIRECTION ( 'NONE',  ( 0.000000000000000000, 0.5877852522924684742, 0.8090169943749507819 ) ) ;
#9657 = VERTEX_POINT ( 'NONE', #598 ) ;
#9658 = AXIS2_PLACEMENT_3D ( 'NONE', #15752, #17284, #13086 ) ;
#9659 = AXIS2_PLACEMENT_3D ( 'NONE', #10393, #1274, #17448 ) ;
#9660 = DIRECTION ( 'NONE',  ( 0.000000000000000000, 0.8090169943749446757, 0.5877852522924769119 ) ) ;
#9661 = DIRECTION ( 'NONE',  ( 0.000000000000000000, -0.4999999999999992228, 0.8660254037844390407 ) ) ;
#9662 = DIRECTION ( 'NONE',  ( 0.000000000000000000, -1.000000000000000000, 0.000000000000000000 ) ) ;
#9663 = CARTESIAN_POINT ( 'NONE',  ( 0.000000000000000000, 14.19907017806868588, 22.07705612348844326 ) ) ;
#9664 = VECTOR ( 'NONE', #1033, 1000.000000000000000 ) ;
#9665 = EDGE_LOOP ( 'NONE', ( #8183, #13464, #11115, #15051 ) ) ;
#9666 = DIRECTION ( 'NONE',  ( 1.000000000000000000, 0.000000000000000000, 0.000000000000000000 ) ) ;
#9667 = VERTEX_POINT ( 'NONE', #9536 ) ;
#9668 = AXIS2_PLACEMENT_3D ( 'NONE', #2008, #5919, #4505 ) ;
#9669 = DIRECTION ( 'NONE',  ( 0.000000000000000000, 0.000000000000000000, 1.000000000000000000 ) ) ;
#9670 = LINE ( 'NONE', #15490, #10427 ) ;
#9671 = DIRECTION ( 'NONE',  ( 0.000000000000000000, 0.000000000000000000, -1.000000000000000000 ) ) ;
#9672 = CIRCLE ( 'NONE', #244, 28.00000000000000711 ) ;
#9673 = ORIENTED_EDGE ( 'NONE', *, *, #4631, .F. ) ;
#9674 = ORIENTED_EDGE ( 'NONE', *, *, #11723, .T. ) ;
#9675 = VECTOR ( 'NONE', #6290, 1000.000000000000000 ) ;
#9676 = DIRECTION ( 'NONE',  ( 0.000000000000000000, 0.000000000000000000, 1.000000000000000000 ) ) ;
#9677 =( NAMED_UNIT ( * ) PLANE_ANGLE_UNIT ( ) SI_UNIT ( $, .RADIAN. ) );
#9678 = ORIENTED_EDGE ( 'NONE', *, *, #18266, .T. ) ;
#9679 = CARTESIAN_POINT ( 'NONE',  ( 10.00000000000000000, -57.83923611457302627, -24.97244012287563919 ) ) ;
#9680 = AXIS2_PLACEMENT_3D ( 'NONE', #1865, #7666, #10710 ) ;
#9681 = ADVANCED_FACE ( 'NONE', ( #13466 ), #409, .F. ) ;
#9682 = LINE ( 'NONE', #12738, #14763 ) ;
#9683 = EDGE_CURVE ( 'NONE', #16517, #8328, #10871, .T. ) ;
#9684 = AXIS2_PLACEMENT_3D ( 'NONE', #9074, #7641, #16700 ) ;
#9685 = VECTOR ( 'NONE', #3615, 1000.000000000000000 ) ;
#9686 = CARTESIAN_POINT ( 'NONE',  ( 0.000000000000000000, -7.813799127872885997, -55.83748330407415494 ) ) ;
#9687 = EDGE_LOOP ( 'NONE', ( #8557, #14281, #10623, #3607 ) ) ;
#9688 = CARTESIAN_POINT ( 'NONE',  ( -6.259644161404860030E-16, -4.618802153517027165, -3.433295621305388234 ) ) ;
#9689 = EDGE_CURVE ( 'NONE', #15464, #17588, #5185, .T. ) ;
#9690 = ORIENTED_EDGE ( 'NONE', *, *, #15356, .F. ) ;
#9691 = CARTESIAN_POINT ( 'NONE',  ( 0.5636800770130377947, 4.293361309317166530, -3.531542292954102713 ) ) ;
#9692 = CARTESIAN_POINT ( 'NONE',  ( 10.00000000000000000, -50.69000562871659810, 24.68609584167141691 ) ) ;
#9693 = DIRECTION ( 'NONE',  ( -1.000000000000000000, -0.000000000000000000, -0.000000000000000000 ) ) ;
#9694 = ORIENTED_EDGE ( 'NONE', *, *, #11334, .F. ) ;
#9695 = CARTESIAN_POINT ( 'NONE',  ( -90.00000000009001155, -38.00000000000000000, -1.301042606982603940E-15 ) ) ;
#9696 = VERTEX_POINT ( 'NONE', #5061 ) ;
#9697 = ADVANCED_FACE ( 'NONE', ( #10965 ), #14982, .T. ) ;
#9698 = LINE ( 'NONE', #15318, #12740 ) ;
#9699 = FACE_OUTER_BOUND ( 'NONE', #10335, .T. ) ;
#9700 = ORIENTED_EDGE ( 'NONE', *, *, #342, .F. ) ;
#9701 = MANIFOLD_SOLID_BREP ( 'M5 Clearance Hole2', #1011 ) ;
#9702 = ORIENTED_EDGE ( 'NONE', *, *, #456, .T. ) ;
#9703 = DIRECTION ( 'NONE',  ( 0.000000000000000000, 0.000000000000000000, 1.000000000000000000 ) ) ;
#9704 = CIRCLE ( 'NONE', #7269, 56.24900000005625600 ) ;
#9706 = EDGE_CURVE ( 'NONE', #4897, #15928, #4573, .T. ) ;
#9705 = VERTEX_POINT ( 'NONE', #694 ) ;
#9707 = DIRECTION ( 'NONE',  ( 0.000000000000000000, 0.000000000000000000, -1.000000000000000000 ) ) ;
#9708 = LINE ( 'NONE', #4092, #5827 ) ;
#9709 = VECTOR ( 'NONE', #12380, 999.9999999999998863 ) ;
#9710 = EDGE_CURVE ( 'NONE', #13795, #9002, #15224, .T. ) ;
#9711 = EDGE_CURVE ( 'NONE', #11347, #8582, #13553, .T. ) ;
#9712 = AXIS2_PLACEMENT_3D ( 'NONE', #1082, #17452, #15842 ) ;
#9713 = ORIENTED_EDGE ( 'NONE', *, *, #10280, .F. ) ;
#9714 = VECTOR ( 'NONE', #8164, 1000.000000000000000 ) ;
#9715 = EDGE_CURVE ( 'NONE', #13493, #5775, #13823, .T. ) ;
#9716 = ORIENTED_EDGE ( 'NONE', *, *, #8308, .T. ) ;
#9717 = DIRECTION ( 'NONE',  ( -1.000000000000000000, 0.000000000000000000, -0.000000000000000000 ) ) ;
#9718 = DIRECTION ( 'NONE',  ( 0.01644736842105263067, 0.9998647328874151752, 0.000000000000000000 ) ) ;
#9720 = EDGE_CURVE ( 'NONE', #7866, #14075, #943, .T. ) ;
#9719 = DIRECTION ( 'NONE',  ( 1.000000000000000000, -0.000000000000000000, -0.000000000000000000 ) ) ;
#9721 = CARTESIAN_POINT ( 'NONE',  ( 0.000000000000000000, 0.000000000000000000, 0.000000000000000000 ) ) ;
#9722 = CARTESIAN_POINT ( 'NONE',  ( 5.000000000000000000, 40.19788616105610402, 48.50907078259395888 ) ) ;
#9723 = DIRECTION ( 'NONE',  ( -0.000000000000000000, 1.000000000000000000, 0.000000000000000000 ) ) ;
#9724 = LINE ( 'NONE', #12956, #1371 ) ;
#9725 = ORIENTED_EDGE ( 'NONE', *, *, #3407, .F. ) ;
#9726 = CARTESIAN_POINT ( 'NONE',  ( -90.00000000009001155, -49.14213562373095812, -1.301042606982603940E-15 ) ) ;
#9727 = CARTESIAN_POINT ( 'NONE',  ( 0.000000000000000000, 0.000000000000000000, 0.000000000000000000 ) ) ;
#9728 = CARTESIAN_POINT ( 'NONE',  ( 10.00000000000000000, -24.46385708179990459, 9.514709542736804693 ) ) ;
#9729 = AXIS2_PLACEMENT_3D ( 'NONE', #1527, #14856, #3144 ) ;
#9730 = DIRECTION ( 'NONE',  ( 0.000000000000000000, 1.000000000000000000, 3.469446951950143595E-15 ) ) ;
#9731 = CONTEXT_DEPENDENT_SHAPE_REPRESENTATION ( #4169, #10273 ) ;
#9732 = VECTOR ( 'NONE', #4836, 1000.000000000000000 ) ;
#9733 = ORIENTED_EDGE ( 'NONE', *, *, #5246, .T. ) ;
#9734 = EDGE_LOOP ( 'NONE', ( #11173, #15029, #17526, #9905 ) ) ;
#9735 = ORIENTED_EDGE ( 'NONE', *, *, #18200, .T. ) ;
#9736 = CARTESIAN_POINT ( 'NONE',  ( 10.00000000000000000, 53.29895248911675765, 18.38754094778260040 ) ) ;
#9737 =( NAMED_UNIT ( * ) PLANE_ANGLE_UNIT ( ) SI_UNIT ( $, .RADIAN. ) );
#9738 = CIRCLE ( 'NONE', #14305, 12.00000000001200640 ) ;
#9739 = SURFACE_STYLE_FILL_AREA ( #3941 ) ;
#9740 = ADVANCED_FACE ( 'NONE', ( #16500 ), #2209, .F. ) ;
#9741 = DIRECTION ( 'NONE',  ( 1.000000000000000000, 0.000000000000000000, 0.000000000000000000 ) ) ;
#9742 = CIRCLE ( 'NONE', #12783, 2.649999999999999467 ) ;
#9743 = DIRECTION ( 'NONE',  ( -1.000000000000000000, 0.000000000000000000, 0.000000000000000000 ) ) ;
#9744 = DIRECTION ( 'NONE',  ( 0.000000000000000000, 0.000000000000000000, 1.000000000000000000 ) ) ;
#9745 = CARTESIAN_POINT ( 'NONE',  ( 0.000000000000000000, 0.000000000000000000, 4.000000000000000000 ) ) ;
#9746 = DIRECTION ( 'NONE',  ( -1.000000000000000000, 0.000000000000000000, 0.000000000000000000 ) ) ;
#9747 = ORIENTED_EDGE ( 'NONE', *, *, #7213, .T. ) ;
#9748 = CARTESIAN_POINT ( 'NONE',  ( -1.250000000000000000, -6.429618962271402616, -1.000000000000000000 ) ) ;
#9749 = VERTEX_POINT ( 'NONE', #790 ) ;
#9750 = DIRECTION ( 'NONE',  ( 0.000000000000000000, -1.000000000000000000, 0.000000000000000000 ) ) ;
#9751 = CARTESIAN_POINT ( 'NONE',  ( 2.595115354961440524, -7.673029147243177306, -1.000000000000000000 ) ) ;
#9752 = ORIENTED_EDGE ( 'NONE', *, *, #14589, .F. ) ;
#9753 = B_SPLINE_CURVE_WITH_KNOTS ( 'NONE', 3,
 ( #16494, #10675, #9244, #6016, #13364, #127 ),
 .UNSPECIFIED., .F., .F.,
 ( 4, 2, 4 ),
 ( 0.002452478801916376308, 0.003676905084148007850, 0.004901331366379639391 ),
 .UNSPECIFIED. ) ;
#9754 = DIRECTION ( 'NONE',  ( 0.000000000000000000, 0.000000000000000000, 1.000000000000000000 ) ) ;
#9755 = APPLICATION_PROTOCOL_DEFINITION ( 'draft international standard', 'automotive_design', 1998, #12791 ) ;
#9756 = DIRECTION ( 'NONE',  ( -1.000000000000000000, 0.000000000000000000, 0.000000000000000000 ) ) ;
#9757 = ORIENTED_EDGE ( 'NONE', *, *, #17263, .T. ) ;
#9758 = APPLICATION_CONTEXT ( 'automotive_design' ) ;
#9759 = AXIS2_PLACEMENT_3D ( 'NONE', #13931, #18593, #11445 ) ;
#9760 = CARTESIAN_POINT ( 'NONE',  ( 5.032868406504335645, -28.36021363089093938, -2.000000000000000000 ) ) ;
#9761 = LINE ( 'NONE', #17104, #8225 ) ;
#9762 = DIRECTION ( 'NONE',  ( -1.000000000000000000, -0.000000000000000000, -0.000000000000000000 ) ) ;
#9763 = EDGE_CURVE ( 'NONE', #15974, #6434, #16134, .T. ) ;
#9764 = CARTESIAN_POINT ( 'NONE',  ( 10.00000000000000000, 0.000000000000000000, 0.000000000000000000 ) ) ;
#9765 = UNCERTAINTY_MEASURE_WITH_UNIT (LENGTH_MEASURE( 1.000000000000000082E-05 ), #8832, 'distance_accuracy_value', 'NONE');
#9766 = DIRECTION ( 'NONE',  ( 0.000000000000000000, 0.000000000000000000, 1.000000000000000000 ) ) ;
#9767 = ORIENTED_EDGE ( 'NONE', *, *, #2146, .T. ) ;
#9768 = CARTESIAN_POINT ( 'NONE',  ( 0.000000000000000000, -29.75305054077462330, -14.27431201565557117 ) ) ;
#9769 = CARTESIAN_POINT ( 'NONE',  ( -79.64793068852898728, -34.99999999999999289, -31.86039329588756530 ) ) ;
#9770 = DIRECTION ( 'NONE',  ( -1.000000000000000000, 0.000000000000000000, 0.000000000000000000 ) ) ;
#9771 = VERTEX_POINT ( 'NONE', #4034 ) ;
#9772 = ORIENTED_EDGE ( 'NONE', *, *, #13675, .F. ) ;
#9773 = DIRECTION ( 'NONE',  ( 0.000000000000000000, 1.000000000000000000, 0.000000000000000000 ) ) ;
#9774 = ORIENTED_EDGE ( 'NONE', *, *, #274, .F. ) ;
#9775 = CARTESIAN_POINT ( 'NONE',  ( -90.72413394419160682, 2.081668171172168513E-14, 4.947285117213266581 ) ) ;
#9776 = EDGE_CURVE ( 'NONE', #5801, #16413, #1835, .T. ) ;
#9777 = VECTOR ( 'NONE', #724, 1000.000000000000000 ) ;
#9778 = EDGE_CURVE ( 'NONE', #7033, #8362, #3060, .T. ) ;
#9779 = DIRECTION ( 'NONE',  ( 0.000000000000000000, 0.8090169943749445647, 0.5877852522924770229 ) ) ;
#9780 = CARTESIAN_POINT ( 'NONE',  ( -36.40576474687247099, 10.00000000000000000, 29.10033635316149514 ) ) ;
#9781 = ORIENTED_EDGE ( 'NONE', *, *, #14953, .T. ) ;
#9782 = CARTESIAN_POINT ( 'NONE',  ( 50.00005079999999680, 0.000000000000000000, 5.000000000000000000 ) ) ;
#9783 = CIRCLE ( 'NONE', #2802, 56.24900000005625600 ) ;
#9784 = EDGE_LOOP ( 'NONE', ( #13564, #10763 ) ) ;
#9786 = LINE ( 'NONE', #17659, #14224 ) ;
#9785 = UNCERTAINTY_MEASURE_WITH_UNIT (LENGTH_MEASURE( 1.000000000000000082E-05 ), #85, 'distance_accuracy_value', 'NONE');
#9787 = CARTESIAN_POINT ( 'NONE',  ( 5.000000000000000000, 29.03656532225586062, -15.68049343255964523 ) ) ;
#9788 = DIRECTION ( 'NONE',  ( 0.000000000000000000, 0.000000000000000000, 1.000000000000000000 ) ) ;
#9789 = ORIENTED_EDGE ( 'NONE', *, *, #16977, .T. ) ;
#9790 = DIRECTION ( 'NONE',  ( -1.000000000000000000, -0.000000000000000000, -0.000000000000000000 ) ) ;
#9791 = ORIENTED_EDGE ( 'NONE', *, *, #17413, .T. ) ;
#9792 = LINE ( 'NONE', #8276, #11208 ) ;
#9793 = DIRECTION ( 'NONE',  ( 1.000000000000000000, 0.000000000000000000, 0.000000000000000000 ) ) ;
#9794 = VERTEX_POINT ( 'NONE', #1269 ) ;
#9795 = ORIENTED_EDGE ( 'NONE', *, *, #12615, .F. ) ;
#9796 = DIRECTION ( 'NONE',  ( -1.000000000000000000, 0.000000000000000000, -0.000000000000000000 ) ) ;
#9797 = SURFACE_STYLE_USAGE ( .BOTH. , #15702 ) ;
#9798 = ORIENTED_EDGE ( 'NONE', *, *, #11534, .T. ) ;
#9799 = DIRECTION ( 'NONE',  ( 0.000000000000000000, 0.000000000000000000, 1.000000000000000000 ) ) ;
#9800 = CARTESIAN_POINT ( 'NONE',  ( 0.000000000000000000, 33.95787273855309252, -45.00825343884985585 ) ) ;
#9801 = CIRCLE ( 'NONE', #1584, 2.649999999999999467 ) ;
#9802 = EDGE_CURVE ( 'NONE', #9572, #2709, #14109, .T. ) ;
#9803 = VERTEX_POINT ( 'NONE', #12588 ) ;
#9804 = PRODUCT ( 'hex flange nut gradea_iso_ISO - 4161 - M5 - N', 'hex flange nut gradea_iso_ISO - 4161 - M5 - N', '', ( #7352 ) ) ;
#9805 = ORIENTED_EDGE ( 'NONE', *, *, #15415, .T. ) ;
#9806 = DIRECTION ( 'NONE',  ( 0.000000000000000000, 1.000000000000000000, 0.000000000000000000 ) ) ;
#9807 = CARTESIAN_POINT ( 'NONE',  ( 10.00000000000000000, 0.000000000000000000, 0.000000000000000000 ) ) ;
#9808 = DIRECTION ( 'NONE',  ( -0.000000000000000000, 1.000000000000000000, -0.000000000000000000 ) ) ;
#9809 = DIRECTION ( 'NONE',  ( -1.000000000000000000, 0.000000000000000000, 0.000000000000000000 ) ) ;
#9810 = VECTOR ( 'NONE', #7894, 1000.000000000000000 ) ;
#9811 = CARTESIAN_POINT ( 'NONE',  ( 10.00000000000000000, -53.92768374110902840, 16.45250512421837641 ) ) ;
#9813 = CIRCLE ( 'NONE', #3126, 41.00000000000000000 ) ;
#9812 = CARTESIAN_POINT ( 'NONE',  ( 3.499999999999999556, -27.60846790388774608, 0.000000000000000000 ) ) ;
#9814 = CARTESIAN_POINT ( 'NONE',  ( 0.000000000000000000, 0.000000000000000000, 0.000000000000000000 ) ) ;
#9815 = ORIENTED_EDGE ( 'NONE', *, *, #12482, .F. ) ;
#9816 = CARTESIAN_POINT ( 'NONE',  ( -1.390230914382372118, -4.043987460488664532, -3.502507215260523665 ) ) ;
#9817 = ADVANCED_FACE ( 'NONE', ( #11353 ), #15456, .T. ) ;
#9818 = EDGE_CURVE ( 'NONE', #11704, #1353, #5635, .T. ) ;
#9819 = DIRECTION ( 'NONE',  ( 0.000000000000000000, 0.000000000000000000, 1.000000000000000000 ) ) ;
#9820 = EDGE_CURVE ( 'NONE', #890, #808, #8499, .T. ) ;
#9821 = FACE_OUTER_BOUND ( 'NONE', #12422, .T. ) ;
#9822 = DIRECTION ( 'NONE',  ( -1.000000000000000000, 0.000000000000000000, 0.000000000000000000 ) ) ;
#9823 = ADVANCED_FACE ( 'NONE', ( #5252 ), #14026, .T. ) ;
#9824 = EDGE_LOOP ( 'NONE', ( #9177, #4228, #8195, #8056 ) ) ;
#9825 = ADVANCED_FACE ( 'NONE', ( #14213 ), #1071, .T. ) ;
#9826 = AXIS2_PLACEMENT_3D ( 'NONE', #7762, #14827, #10714 ) ;
#9827 = EDGE_LOOP ( 'NONE', ( #3248, #9206 ) ) ;
#9828 = AXIS2_PLACEMENT_3D ( 'NONE', #5337, #8491, #9730 ) ;
#9829 = ORIENTED_EDGE ( 'NONE', *, *, #4688, .T. ) ;
#9830 = ADVANCED_FACE ( 'NONE', ( #899 ), #17267, .T. ) ;
#9831 = CARTESIAN_POINT ( 'NONE',  ( 10.00000000000000000, -7.813799127872885997, -55.83748330407415494 ) ) ;
#9832 = SURFACE_STYLE_FILL_AREA ( #14312 ) ;
#9833 = SURFACE_STYLE_FILL_AREA ( #11262 ) ;
#9834 = DIRECTION ( 'NONE',  ( 0.000000000000000000, 0.000000000000000000, 1.000000000000000000 ) ) ;
#9835 = CARTESIAN_POINT ( 'NONE',  ( 0.2500000000000002220, 0.000000000000000000, 0.000000000000000000 ) ) ;
#9836 = CARTESIAN_POINT ( 'NONE',  ( 0.000000000000000000, 11.24999999999999467, 0.000000000000000000 ) ) ;
#9837 = CARTESIAN_POINT ( 'NONE',  ( 10.00000000000000000, 0.000000000000000000, 0.000000000000000000 ) ) ;
#9838 = ORIENTED_EDGE ( 'NONE', *, *, #7118, .T. ) ;
#9839 = DIRECTION ( 'NONE',  ( 0.000000000000000000, 0.000000000000000000, 1.000000000000000000 ) ) ;
#9840 = ORIENTED_EDGE ( 'NONE', *, *, #7377, .T. ) ;
#9841 = EDGE_CURVE ( 'NONE', #17232, #139, #15345, .T. ) ;
#9842 = AXIS2_PLACEMENT_3D ( 'NONE', #517, #10695, #18123 ) ;
#9843 = LINE ( 'NONE', #5362, #6490 ) ;
#9844 = CARTESIAN_POINT ( 'NONE',  ( 10.00000000000000000, -56.37237871411032586, -1.017308535512989609 ) ) ;
#9845 = VERTEX_POINT ( 'NONE', #6695 ) ;
#9846 = PLANE ( 'NONE',  #14184 ) ;
#9847 = CARTESIAN_POINT ( 'NONE',  ( 45.00000000000000000, -14.99999999999999289, 1.318389841742373392E-13 ) ) ;
#9848 = CARTESIAN_POINT ( 'NONE',  ( 10.00000000000000000, 0.000000000000000000, 0.000000000000000000 ) ) ;
#9849 = EDGE_LOOP ( 'NONE', ( #8549, #3745, #18163, #7310 ) ) ;
#9850 = ADVANCED_FACE ( 'NONE', ( #9919 ), #15737, .T. ) ;
#9851 = MECHANICAL_DESIGN_GEOMETRIC_PRESENTATION_REPRESENTATION (  '', ( #14113 ), #12278 ) ;
#9852 = DIRECTION ( 'NONE',  ( 0.000000000000000000, 0.5877852522924685852, 0.8090169943749505599 ) ) ;
#9853 = DIRECTION ( 'NONE',  ( -1.000000000000000000, -0.000000000000000000, -0.000000000000000000 ) ) ;
#9854 = MANIFOLD_SOLID_BREP ( 'M5 Clearance Hole1', #9519 ) ;
#9855 = DIRECTION ( 'NONE',  ( -1.000000000000000000, 0.000000000000000000, 0.000000000000000000 ) ) ;
#9856 = CARTESIAN_POINT ( 'NONE',  ( -90.00000000009001155, -34.99999999999999289, 10.00000000000000711 ) ) ;
#9857 = CARTESIAN_POINT ( 'NONE',  ( 10.00000000000000000, -20.32630374611196800, 16.60877409751161693 ) ) ;
#9858 = VERTEX_POINT ( 'NONE', #1355 ) ;
#9859 = FACE_OUTER_BOUND ( 'NONE', #17568, .T. ) ;
#9860 = CARTESIAN_POINT ( 'NONE',  ( 4.999999999999999112, -5.876895005582878362, 62.72529079327805590 ) ) ;
#9861 = CARTESIAN_POINT ( 'NONE',  ( -4.000000000000000000, 2.309401076758498483, -3.433295621305379353 ) ) ;
#9862 = EDGE_LOOP ( 'NONE', ( #6836, #11382, #11230, #18737 ) ) ;
#9863 = ORIENTED_EDGE ( 'NONE', *, *, #2828, .F. ) ;
#9864 = APPLICATION_CONTEXT ( 'automotive_design' ) ;
#9865 = FACE_BOUND ( 'NONE', #9874, .T. ) ;
#9866 = ORIENTED_EDGE ( 'NONE', *, *, #8794, .F. ) ;
#9867 = CARTESIAN_POINT ( 'NONE',  ( 13.90576474687263264, 10.00000000000000000, -42.79754323328189969 ) ) ;
#9868 = EDGE_CURVE ( 'NONE', #15243, #6017, #1246, .T. ) ;
#9869 = DIRECTION ( 'NONE',  ( -1.000000000000000000, -0.000000000000000000, -0.000000000000000000 ) ) ;
#9870 = DIRECTION ( 'NONE',  ( 0.000000000000000000, 0.000000000000000000, 1.000000000000000000 ) ) ;
#9871 = EDGE_LOOP ( 'NONE', ( #17260, #6468, #6767, #6524 ) ) ;
#9872 = CARTESIAN_POINT ( 'NONE',  ( 0.000000000000000000, -16.10733642026445978, -53.89344778774828626 ) ) ;
#9873 = MECHANICAL_DESIGN_GEOMETRIC_PRESENTATION_REPRESENTATION (  '', ( #15961 ), #14734 ) ;
#9874 = EDGE_LOOP ( 'NONE', ( #16021, #6837 ) ) ;
#9875 = DIRECTION ( 'NONE',  ( 0.000000000000000000, 0.000000000000000000, 1.000000000000000000 ) ) ;
#9876 = CARTESIAN_POINT ( 'NONE',  ( 0.000000000000000000, 5.876895005583346432, -62.72529079327799906 ) ) ;
#9877 = DIRECTION ( 'NONE',  ( 0.000000000000000000, 0.000000000000000000, 1.000000000000000000 ) ) ;
#9878 = AXIS2_PLACEMENT_3D ( 'NONE', #10732, #9302, #5012 ) ;
#9879 = ORIENTED_EDGE ( 'NONE', *, *, #9802, .F. ) ;
#9880 = DIRECTION ( 'NONE',  ( -1.000000000000000000, 0.000000000000000000, -0.000000000000000000 ) ) ;
#9881 = EDGE_LOOP ( 'NONE', ( #13812, #18720, #18643, #3631 ) ) ;
#9882 = EDGE_CURVE ( 'NONE', #15207, #7869, #1625, .T. ) ;
#9883 = CYLINDRICAL_SURFACE ( 'NONE', #2403, 24.00000000002400213 ) ;
#9884 = FACE_OUTER_BOUND ( 'NONE', #10646, .T. ) ;
#9885 = ORIENTED_EDGE ( 'NONE', *, *, #11861, .F. ) ;
#9886 = VERTEX_POINT ( 'NONE', #17535 ) ;
#9887 = CARTESIAN_POINT ( 'NONE',  ( -4.249769933734879324, -30.10148593525447680, -2.000000000000000000 ) ) ;
#9888 = EDGE_CURVE ( 'NONE', #16606, #18250, #10384, .T. ) ;
#9889 = VERTEX_POINT ( 'NONE', #300 ) ;
#9890 = LINE ( 'NONE', #2467, #9095 ) ;
#9891 = LINE ( 'NONE', #17144, #11612 ) ;
#9892 = VERTEX_POINT ( 'NONE', #1550 ) ;
#9893 = CIRCLE ( 'NONE', #1675, 30.00000000000000000 ) ;
#9894 = ORIENTED_EDGE ( 'NONE', *, *, #4993, .T. ) ;
#9895 = EDGE_LOOP ( 'NONE', ( #1773, #18267 ) ) ;
#9896 = DIRECTION ( 'NONE',  ( 0.000000000000000000, 0.000000000000000000, 1.000000000000000000 ) ) ;
#9897 = DIRECTION ( 'NONE',  ( -1.000000000000000000, -0.000000000000000000, -0.000000000000000000 ) ) ;
#9898 = CARTESIAN_POINT ( 'NONE',  ( 0.000000000000000000, 0.000000000000000000, 0.000000000000000000 ) ) ;
#9899 = DIRECTION ( 'NONE',  ( -1.000000000000000000, 0.000000000000000000, 0.000000000000000000 ) ) ;
#9900 =( LENGTH_UNIT ( ) NAMED_UNIT ( * ) SI_UNIT ( .MILLI., .METRE. ) );
#9901 = DIRECTION ( 'NONE',  ( 0.000000000000000000, 0.000000000000000000, -1.000000000000000000 ) ) ;
#9902 = DIRECTION ( 'NONE',  ( 0.000000000000000000, 0.000000000000000000, 1.000000000000000000 ) ) ;
#9903 = AXIS2_PLACEMENT_3D ( 'NONE', #17860, #12230, #18043 ) ;
#9904 = CARTESIAN_POINT ( 'NONE',  ( 5.021051876504148963E-15, -30.00000000000000000, 41.00000000000000000 ) ) ;
#9905 = ORIENTED_EDGE ( 'NONE', *, *, #16567, .T. ) ;
#9906 = CARTESIAN_POINT ( 'NONE',  ( 0.1410422978106145031, -4.700232962125109104, -3.687027686973628704 ) ) ;
#9907 = AXIS2_PLACEMENT_3D ( 'NONE', #17724, #17812, #122 ) ;
#9908 = FACE_OUTER_BOUND ( 'NONE', #1779, .T. ) ;
#9909 = CARTESIAN_POINT ( 'NONE',  ( -12.69999999999999929, 0.000000000000000000, 0.000000000000000000 ) ) ;
#9910 = EDGE_LOOP ( 'NONE', ( #15012, #3871 ) ) ;
#9911 = EDGE_LOOP ( 'NONE', ( #15492, #14313 ) ) ;
#9912 = VECTOR ( 'NONE', #5105, 1000.000000000000000 ) ;
#9913 = AXIS2_PLACEMENT_3D ( 'NONE', #15074, #4600, #6308 ) ;
#9914 = AXIS2_PLACEMENT_3D ( 'NONE', #9331, #15160, #2106 ) ;
#9915 = EDGE_CURVE ( 'NONE', #1879, #3205, #7249, .T. ) ;
#9916 = VERTEX_POINT ( 'NONE', #17361 ) ;
#9917 = DIRECTION ( 'NONE',  ( 0.000000000000000000, 0.000000000000000000, 1.000000000000000000 ) ) ;
#9918 = ADVANCED_FACE ( 'NONE', ( #4488 ), #14762, .T. ) ;
#9919 = FACE_OUTER_BOUND ( 'NONE', #2545, .T. ) ;
#9920 = VERTEX_POINT ( 'NONE', #11822 ) ;
#9921 = DIRECTION ( 'NONE',  ( 1.000000000000000000, 0.000000000000000000, 0.000000000000000000 ) ) ;
#9922 = FACE_OUTER_BOUND ( 'NONE', #15875, .T. ) ;
#9923 = EDGE_CURVE ( 'NONE', #1081, #1734, #10362, .T. ) ;
#9924 = FACE_OUTER_BOUND ( 'NONE', #17870, .T. ) ;
#9925 = DIRECTION ( 'NONE',  ( -1.000000000000000000, 0.000000000000000000, 0.000000000000000000 ) ) ;
#9926 = CIRCLE ( 'NONE', #8697, 0.2000000000000000944 ) ;
#9927 = CARTESIAN_POINT ( 'NONE',  ( 0.000000000000000000, 10.00000000000000000, 0.000000000000000000 ) ) ;
#9928 = VERTEX_POINT ( 'NONE', #14672 ) ;
#9929 = DIRECTION ( 'NONE',  ( 0.000000000000000000, 0.000000000000000000, 1.000000000000000000 ) ) ;
#9930 = AXIS2_PLACEMENT_3D ( 'NONE', #2571, #17160, #15538 ) ;
#9931 = ORIENTED_EDGE ( 'NONE', *, *, #8091, .T. ) ;
#9932 = ADVANCED_FACE ( 'NONE', ( #7426 ), #204, .T. ) ;
#9933 = CIRCLE ( 'NONE', #13867, 24.00000000002399858 ) ;
#9934 = DIRECTION ( 'NONE',  ( 1.000000000000000000, 0.000000000000000000, 0.000000000000000000 ) ) ;
#9935 = DIRECTION ( 'NONE',  ( 1.000000000000000000, 0.000000000000000000, 0.000000000000000000 ) ) ;
#9936 = ORIENTED_EDGE ( 'NONE', *, *, #18405, .F. ) ;
#9937 = AXIS2_PLACEMENT_3D ( 'NONE', #7923, #3829, #13740 ) ;
#9938 = CIRCLE ( 'NONE', #16927, 2.100000000000000089 ) ;
#9939 = CARTESIAN_POINT ( 'NONE',  ( -90.38553543446691663, 1.821459649775647449E-14, -4.784491867360616268 ) ) ;
#9940 = APPLICATION_PROTOCOL_DEFINITION ( 'draft international standard', 'automotive_design', 1998, #7187 ) ;
#9941 = DIRECTION ( 'NONE',  ( 0.000000000000000000, 1.000000000000000000, 0.000000000000000000 ) ) ;
#9942 = ORIENTED_EDGE ( 'NONE', *, *, #2289, .F. ) ;
#9943 = EDGE_CURVE ( 'NONE', #7667, #7777, #16199, .T. ) ;
#9944 = ADVANCED_FACE ( 'NONE', ( #4392 ), #7527, .F. ) ;
#9945 = CONICAL_SURFACE ( 'NONE', #1726, 2.055000000000000160, 0.7853981633974639331 ) ;
#9946 = DIRECTION ( 'NONE',  ( -1.000000000000000000, 2.031314180040284764E-16, 0.000000000000000000 ) ) ;
#9947 = EDGE_CURVE ( 'NONE', #7125, #13289, #8543, .T. ) ;
#9948 = DIRECTION ( 'NONE',  ( -1.000000000000000000, -0.000000000000000000, -0.000000000000000000 ) ) ;
#9949 = CIRCLE ( 'NONE', #18461, 24.00000000002399503 ) ;
#9950 = CIRCLE ( 'NONE', #12065, 12.00000000001200462 ) ;
#9951 = CARTESIAN_POINT ( 'NONE',  ( 0.000000000000000000, 0.000000000000000000, 0.000000000000000000 ) ) ;
#9952 = LINE ( 'NONE', #15767, #3974 ) ;
#9953 = EDGE_CURVE ( 'NONE', #18738, #12029, #12495, .T. ) ;
#9954 = PLANE ( 'NONE',  #6032 ) ;
#9955 = ORIENTED_EDGE ( 'NONE', *, *, #938, .F. ) ;
#9956 = ADVANCED_FACE ( 'NONE', ( #10022 ), #7338, .T. ) ;
#9957 = CARTESIAN_POINT ( 'NONE',  ( -97.50000000009001155, -10.00000000000001599, -1.496198998029995330E-15 ) ) ;
#9958 = DIRECTION ( 'NONE',  ( -1.000000000000000000, -0.000000000000000000, 0.000000000000000000 ) ) ;
#9959 = CARTESIAN_POINT ( 'NONE',  ( 10.00000000000000000, 0.000000000000000000, 0.000000000000000000 ) ) ;
#9960 = AXIS2_PLACEMENT_3D ( 'NONE', #13227, #17087, #3943 ) ;
#9961 = ORIENTED_EDGE ( 'NONE', *, *, #4574, .T. ) ;
#9962 = ORIENTED_EDGE ( 'NONE', *, *, #5033, .F. ) ;
#9963 = DIRECTION ( 'NONE',  ( 0.000000000000000000, 0.000000000000000000, 1.000000000000000000 ) ) ;
#9964 = ORIENTED_EDGE ( 'NONE', *, *, #11567, .T. ) ;
#9965 = DIRECTION ( 'NONE',  ( 0.000000000000000000, 0.000000000000000000, 1.000000000000000000 ) ) ;
#9966 = VECTOR ( 'NONE', #8540, 1000.000000000000000 ) ;
#9967 = FACE_OUTER_BOUND ( 'NONE', #1343, .T. ) ;
#9968 = CIRCLE ( 'NONE', #18803, 5.000000000000000000 ) ;
#9969 = DIRECTION ( 'NONE',  ( 0.000000000000000000, -0.8090169943749530024, 0.5877852522924653655 ) ) ;
#9970 = ORIENTED_EDGE ( 'NONE', *, *, #18570, .T. ) ;
#9971 = DIRECTION ( 'NONE',  ( 0.000000000000000000, 0.000000000000000000, 1.000000000000000000 ) ) ;
#9972 = VECTOR ( 'NONE', #16325, 1000.000000000000000 ) ;
#9973 = CIRCLE ( 'NONE', #1168, 56.24900000005625600 ) ;
#9974 = EDGE_LOOP ( 'NONE', ( #2988, #17133 ) ) ;
#9975 = AXIS2_PLACEMENT_3D ( 'NONE', #4888, #2031, #10687 ) ;
#9976 = DIRECTION ( 'NONE',  ( -1.000000000000000000, -0.000000000000000000, 0.000000000000000000 ) ) ;
#9977 = ORIENTED_EDGE ( 'NONE', *, *, #10210, .T. ) ;
#9978 = LINE ( 'NONE', #1317, #18414 ) ;
#9979 = ADVANCED_FACE ( 'NONE', ( #7152 ), #18779, .T. ) ;
#9980 = ORIENTED_EDGE ( 'NONE', *, *, #9064, .F. ) ;
#9981 = CARTESIAN_POINT ( 'NONE',  ( 0.000000000000000000, -54.20017844242489247, -32.11449294037253566 ) ) ;
#9982 = DIRECTION ( 'NONE',  ( -1.000000000000000000, -0.000000000000000000, 0.000000000000000000 ) ) ;
#9983 = ORIENTED_EDGE ( 'NONE', *, *, #8982, .F. ) ;
#9984 = VERTEX_POINT ( 'NONE', #4309 ) ;
#9985 = DIRECTION ( 'NONE',  ( 0.000000000000000000, -1.000000000000000000, 0.000000000000000000 ) ) ;
#9986 = ORIENTED_EDGE ( 'NONE', *, *, #8496, .T. ) ;
#9987 = DIRECTION ( 'NONE',  ( -1.000000000000000000, -0.000000000000000000, -0.000000000000000000 ) ) ;
#9988 = CARTESIAN_POINT ( 'NONE',  ( 0.000000000000000000, -7.813799127873676476, 55.83748330407405547 ) ) ;
#9989 = CIRCLE ( 'NONE', #15769, 63.00000000006298961 ) ;
#9990 = AXIS2_PLACEMENT_3D ( 'NONE', #13921, #887, #6684 ) ;
#9991 = CIRCLE ( 'NONE', #16388, 27.50000000000000000 ) ;
#9992 = EDGE_CURVE ( 'NONE', #10416, #13348, #2873, .T. ) ;
#9993 = DIRECTION ( 'NONE',  ( -0.000000000000000000, 1.000000000000000000, -0.000000000000000000 ) ) ;
#9994 = ORIENTED_EDGE ( 'NONE', *, *, #11796, .T. ) ;
#9995 = EDGE_CURVE ( 'NONE', #2244, #2800, #4298, .T. ) ;
#9996 = VECTOR ( 'NONE', #5074, 1000.000000000000000 ) ;
#9997 = VERTEX_POINT ( 'NONE', #116 ) ;
#9998 = CYLINDRICAL_SURFACE ( 'NONE', #4769, 2.649999999999999467 ) ;
#9999 = DIRECTION ( 'NONE',  ( -1.000000000000000000, 0.000000000000000000, -0.000000000000000000 ) ) ;
#10000 = CARTESIAN_POINT ( 'NONE',  ( 0.000000000000000000, -13.75000000000000355, 0.000000000000000000 ) ) ;
#10001 = CARTESIAN_POINT ( 'NONE',  ( -56.50000000009000445, -30.00000000000000000, -2.649999999999610889 ) ) ;
#10002 = AXIS2_PLACEMENT_3D ( 'NONE', #5904, #6091, #14667 ) ;
#10003 = LINE ( 'NONE', #15819, #15477 ) ;
#10004 = CARTESIAN_POINT ( 'NONE',  ( 2.250000000000000000, -27.60846790388774608, 0.000000000000000000 ) ) ;
#10005 = VECTOR ( 'NONE', #14295, 1000.000000000000000 ) ;
#10006 = DIRECTION ( 'NONE',  ( 0.000000000000000000, 0.000000000000000000, 1.000000000000000000 ) ) ;
#10007 = EDGE_LOOP ( 'NONE', ( #12435, #13843, #5853, #11958 ) ) ;
#10008 = CIRCLE ( 'NONE', #6966, 0.7500000000000000000 ) ;
#10009 = DIRECTION ( 'NONE',  ( 0.000000000000000000, 0.5877852522924744694, -0.8090169943749464521 ) ) ;
#10010 = FACE_OUTER_BOUND ( 'NONE', #1406, .T. ) ;
#10011 = ORIENTED_EDGE ( 'NONE', *, *, #1793, .T. ) ;
#10012 = CYLINDRICAL_SURFACE ( 'NONE', #8771, 26.24900000002624978 ) ;
#10013 = CARTESIAN_POINT ( 'NONE',  ( -10.00000000000000000, 0.000000000000000000, 0.000000000000000000 ) ) ;
#10014 = ORIENTED_EDGE ( 'NONE', *, *, #6952, .T. ) ;
#10015 = AXIS2_PLACEMENT_3D ( 'NONE', #9526, #17920, #10674 ) ;
#10016 = ADVANCED_FACE ( 'NONE', ( #12545 ), #18261, .T. ) ;
#10017 = AXIS2_PLACEMENT_3D ( 'NONE', #3904, #18568, #1045 ) ;
#10018 = EDGE_CURVE ( 'NONE', #6670, #8465, #14632, .T. ) ;
#10019 = VERTEX_POINT ( 'NONE', #12095 ) ;
#10020 = ADVANCED_FACE ( 'NONE', ( #6286 ), #11989, .T. ) ;
#10021 = DIRECTION ( 'NONE',  ( -1.000000000000000000, -0.000000000000000000, 0.000000000000000000 ) ) ;
#10022 = FACE_OUTER_BOUND ( 'NONE', #11073, .T. ) ;
#10023 = ORIENTED_EDGE ( 'NONE', *, *, #10061, .T. ) ;
#10024 = CARTESIAN_POINT ( 'NONE',  ( 4.000000000000000000, 0.3987449864460005378, -0.01220643443059817035 ) ) ;
#10025 = CARTESIAN_POINT ( 'NONE',  ( 4.000000000000000000, -2.309401076758516691, -0.4999999999999995559 ) ) ;
#10026 = CIRCLE ( 'NONE', #1812, 56.24900000005625600 ) ;
#10027 = CARTESIAN_POINT ( 'NONE',  ( 0.000000000000000000, 14.27431201565567243, -29.75305054077457356 ) ) ;
#10028 = CARTESIAN_POINT ( 'NONE',  ( -90.40159941089927997, 1.000000000000014655, -4.983845695167307355 ) ) ;
#10029 = ORIENTED_EDGE ( 'NONE', *, *, #14958, .T. ) ;
#10030 = LINE ( 'NONE', #13081, #891 ) ;
#10031 = ORIENTED_EDGE ( 'NONE', *, *, #12446, .F. ) ;
#10032 = VECTOR ( 'NONE', #15078, 1000.000000000000000 ) ;
#10033 = VECTOR ( 'NONE', #7852, 1000.000000000000000 ) ;
#10034 = DIRECTION ( 'NONE',  ( 0.000000000000000000, 0.000000000000000000, 1.000000000000000000 ) ) ;
#10035 = VERTEX_POINT ( 'NONE', #6736 ) ;
#10036 = EDGE_CURVE ( 'NONE', #7525, #941, #6187, .T. ) ;
#10037 = APPLICATION_PROTOCOL_DEFINITION ( 'draft international standard', 'automotive_design', 1998, #13155 ) ;
#10039 = EDGE_CURVE ( 'NONE', #17362, #9048, #17910, .T. ) ;
#10038 = FACE_OUTER_BOUND ( 'NONE', #9665, .T. ) ;
#10040 = ORIENTED_EDGE ( 'NONE', *, *, #5179, .F. ) ;
#10041 = CIRCLE ( 'NONE', #4269, 12.00000000001200284 ) ;
#10042 = ORIENTED_EDGE ( 'NONE', *, *, #13333, .T. ) ;
#10043 = VECTOR ( 'NONE', #5187, 1000.000000000000000 ) ;
#10044 = DIRECTION ( 'NONE',  ( 1.000000000000000000, 0.000000000000000000, 0.000000000000000000 ) ) ;
#10045 = LINE ( 'NONE', #2804, #18559 ) ;
#10046 = DIRECTION ( 'NONE',  ( 0.000000000000000000, 0.9510565162951523099, 0.3090169943749516701 ) ) ;
#10047 = CARTESIAN_POINT ( 'NONE',  ( -11.25000000000000533, 0.000000000000000000, 0.000000000000000000 ) ) ;
#10048 = FACE_BOUND ( 'NONE', #16113, .T. ) ;
#10049 = VERTEX_POINT ( 'NONE', #10665 ) ;
#10050 = DIRECTION ( 'NONE',  ( 0.000000000000000000, 0.000000000000000000, 1.000000000000000000 ) ) ;
#10051 = CARTESIAN_POINT ( 'NONE',  ( 10.00000000000000000, 0.000000000000000000, 0.000000000000000000 ) ) ;
#10052 = CARTESIAN_POINT ( 'NONE',  ( 0.000000000000000000, 0.000000000000000000, -1.000000000000000000 ) ) ;
#10053 = VERTEX_POINT ( 'NONE', #10467 ) ;
#10054 = ORIENTED_EDGE ( 'NONE', *, *, #9776, .F. ) ;
#10055 = EDGE_CURVE ( 'NONE', #2269, #7704, #6968, .T. ) ;
#10056 = EDGE_CURVE ( 'NONE', #1945, #7339, #3884, .T. ) ;
#10057 = FACE_BOUND ( 'NONE', #12011, .T. ) ;
#10058 = CIRCLE ( 'NONE', #5799, 24.00000000002399858 ) ;
#10059 = FILL_AREA_STYLE_COLOUR ( '', #12296 ) ;
#10060 = EDGE_CURVE ( 'NONE', #16942, #2331, #15239, .T. ) ;
#10061 = EDGE_CURVE ( 'NONE', #484, #14748, #15502, .T. ) ;
#10062 = ORIENTED_EDGE ( 'NONE', *, *, #3537, .F. ) ;
#10063 = EDGE_CURVE ( 'NONE', #18755, #12204, #1556, .T. ) ;
#10064 = CARTESIAN_POINT ( 'NONE',  ( 0.000000000000000000, -26.50000000000000000, 0.000000000000000000 ) ) ;
#10065 = DIRECTION ( 'NONE',  ( 0.000000000000000000, -0.9510565162951502005, -0.3090169943749581649 ) ) ;
#10066 = ORIENTED_EDGE ( 'NONE', *, *, #10684, .T. ) ;
#10068 = VECTOR ( 'NONE', #17038, 1000.000000000000000 ) ;
#10067 = CARTESIAN_POINT ( 'NONE',  ( 10.00000000000000000, 0.000000000000000000, 0.000000000000000000 ) ) ;
#10069 = ADVANCED_FACE ( 'NONE', ( #14069 ), #1816, .F. ) ;
#10070 = ORIENTED_EDGE ( 'NONE', *, *, #10156, .F. ) ;
#10071 = FACE_BOUND ( 'NONE', #15340, .T. ) ;
#10072 = VERTEX_POINT ( 'NONE', #8066 ) ;
#10073 = CARTESIAN_POINT ( 'NONE',  ( 10.00000000000000000, -33.95787273855277988, 45.00825343885009033 ) ) ;
#10074 = VERTEX_POINT ( 'NONE', #9046 ) ;
#10075 = CARTESIAN_POINT ( 'NONE',  ( 2.500000000000000000, 0.000000000000000000, 0.000000000000000000 ) ) ;
#10076 = FACE_OUTER_BOUND ( 'NONE', #4, .T. ) ;
#10077 = ORIENTED_EDGE ( 'NONE', *, *, #2740, .F. ) ;
#10078 = ORIENTED_EDGE ( 'NONE', *, *, #4993, .F. ) ;
#10079 = EDGE_CURVE ( 'NONE', #1489, #1871, #14869, .T. ) ;
#10080 = CARTESIAN_POINT ( 'NONE',  ( -10.00000000000000000, 0.000000000000000000, 0.000000000000000000 ) ) ;
#10081 = ORIENTED_EDGE ( 'NONE', *, *, #3033, .F. ) ;
#10082 = LINE ( 'NONE', #4188, #8791 ) ;
#10083 = VECTOR ( 'NONE', #15284, 1000.000000000000000 ) ;
#10084 = EDGE_CURVE ( 'NONE', #1683, #11596, #11879, .T. ) ;
#10085 = VECTOR ( 'NONE', #11357, 1000.000000000000000 ) ;
#10086 = CARTESIAN_POINT ( 'NONE',  ( -10.00000000000000000, 0.000000000000000000, 0.000000000000000000 ) ) ;
#10087 = AXIS2_PLACEMENT_3D ( 'NONE', #9513, #16762, #15518 ) ;
#10088 = ORIENTED_EDGE ( 'NONE', *, *, #1538, .F. ) ;
#10089 = ORIENTED_EDGE ( 'NONE', *, *, #12971, .T. ) ;
#10090 = CARTESIAN_POINT ( 'NONE',  ( 10.04305231718579705, -30.00000000000000000, 28.25933677959249835 ) ) ;
#10091 = CARTESIAN_POINT ( 'NONE',  ( 10.00000000000000000, -13.40641754777648487, -24.79895094899273644 ) ) ;
#10092 = CARTESIAN_POINT ( 'NONE',  ( -10.00000000000000000, 0.000000000000000000, 0.000000000000000000 ) ) ;
#10093 = B_SPLINE_CURVE_WITH_KNOTS ( 'NONE', 3,
 ( #14909, #4615, #6135, #7742, #17755, #15000, #11946, #7570 ),
 .UNSPECIFIED., .F., .F.,
 ( 4, 2, 2, 4 ),
 ( 2.465131517071352357E-07, 0.001183067374689843057, 0.001774477805458910071, 0.002365888236227977302 ),
 .UNSPECIFIED. ) ;
#10094 = DIRECTION ( 'NONE',  ( 0.000000000000000000, 0.000000000000000000, -1.000000000000000000 ) ) ;
#10095 = DIRECTION ( 'NONE',  ( -1.000000000000000000, -0.000000000000000000, 0.000000000000000000 ) ) ;
#10096 = DIRECTION ( 'NONE',  ( -1.000000000000000000, -0.000000000000000000, -0.000000000000000000 ) ) ;
#10097 = FACE_OUTER_BOUND ( 'NONE', #6611, .T. ) ;
#10098 = CARTESIAN_POINT ( 'NONE',  ( 0.000000000000000000, 32.70783759231086663, -4.381479206523104963 ) ) ;
#10099 = EDGE_LOOP ( 'NONE', ( #14743, #6823 ) ) ;
#10100 = DIRECTION ( 'NONE',  ( 0.000000000000000000, -0.9876883405951393247, 0.1564344650402205161 ) ) ;
#10101 = DIRECTION ( 'NONE',  ( -1.000000000000000000, -0.000000000000000000, -0.000000000000000000 ) ) ;
#10102 = VECTOR ( 'NONE', #5257, 1000.000000000000000 ) ;
#10103 = VECTOR ( 'NONE', #16854, 1000.000000000000000 ) ;
#10104 = VERTEX_POINT ( 'NONE', #382 ) ;
#10105 = DIRECTION ( 'NONE',  ( 0.000000000000000000, 0.000000000000000000, 1.000000000000000000 ) ) ;
#10106 = DIRECTION ( 'NONE',  ( -1.000000000000000000, -0.000000000000000000, -0.000000000000000000 ) ) ;
#10107 = EDGE_LOOP ( 'NONE', ( #17989, #6743 ) ) ;
#10108 = MANIFOLD_SOLID_BREP ( 'M5 Clearance Hole4', #17734 ) ;
#10109 = EDGE_CURVE ( 'NONE', #18729, #8150, #15595, .T. ) ;
#10110 = ORIENTED_EDGE ( 'NONE', *, *, #12732, .T. ) ;
#10112 = CARTESIAN_POINT ( 'NONE',  ( 0.000000000000000000, -26.50000000000000000, 0.000000000000000000 ) ) ;
#10111 = AXIS2_PLACEMENT_3D ( 'NONE', #5329, #6765, #14299 ) ;
#10113 = CARTESIAN_POINT ( 'NONE',  ( 0.000000000000000000, 32.31183295104772668, 46.20417134726143615 ) ) ;
#10114 = ORIENTED_EDGE ( 'NONE', *, *, #18543, .F. ) ;
#10115 = PRESENTATION_STYLE_ASSIGNMENT (( #2875 ) ) ;
#10116 = APPLICATION_CONTEXT ( 'automotive_design' ) ;
#10117 = FACE_BOUND ( 'NONE', #6077, .T. ) ;
#10118 = DIRECTION ( 'NONE',  ( -0.000000000000000000, 1.000000000000000000, -0.000000000000000000 ) ) ;
#10119 = DIRECTION ( 'NONE',  ( 0.000000000000000000, 0.000000000000000000, -1.000000000000000000 ) ) ;
#10120 = DIRECTION ( 'NONE',  ( -0.000000000000000000, -1.000000000000000000, -0.000000000000000000 ) ) ;
#10121 = ORIENTED_EDGE ( 'NONE', *, *, #16059, .T. ) ;
#10122 = DIRECTION ( 'NONE',  ( 0.000000000000000000, 1.000000000000000000, 0.000000000000000000 ) ) ;
#10123 = EDGE_LOOP ( 'NONE', ( #10263, #7017, #1754, #1850 ) ) ;
#10124 = EDGE_CURVE ( 'NONE', #2703, #4666, #18586, .T. ) ;
#10125 = PRODUCT_DEFINITION_SHAPE ( 'NONE', 'NONE',  #18836 ) ;
#10126 = DIRECTION ( 'NONE',  ( -1.000000000000000000, -0.000000000000000000, -0.000000000000000000 ) ) ;
#10127 = ORIENTED_EDGE ( 'NONE', *, *, #12971, .F. ) ;
#10128 = PRODUCT_CONTEXT ( 'NONE', #4630, 'mechanical' ) ;
#10129 = ADVANCED_FACE ( 'NONE', ( #7019 ), #12834, .F. ) ;
#10130 = CIRCLE ( 'NONE', #4049, 56.24900000005625600 ) ;
#10131 = ORIENTED_EDGE ( 'NONE', *, *, #747, .F. ) ;
#10132 = AXIS2_PLACEMENT_3D ( 'NONE', #17566, #2543, #12643 ) ;
#10133 = DIRECTION ( 'NONE',  ( -1.000000000000000000, -0.000000000000000000, 0.000000000000000000 ) ) ;
#10134 = DIRECTION ( 'NONE',  ( 1.000000000000000000, -0.000000000000000000, -0.000000000000000000 ) ) ;
#10135 = DIRECTION ( 'NONE',  ( 0.000000000000000000, 0.000000000000000000, 1.000000000000000000 ) ) ;
#10136 = CYLINDRICAL_SURFACE ( 'NONE', #10376, 24.00000000002399858 ) ;
#10137 = AXIS2_PLACEMENT_3D ( 'NONE', #18535, #15670, #8438 ) ;
#10138 = AXIS2_PLACEMENT_3D ( 'NONE', #9223, #1988, #2096 ) ;
#10139 = CARTESIAN_POINT ( 'NONE',  ( -11.15000000000000391, 0.000000000000000000, 25.10000000000000142 ) ) ;
#10140 = VERTEX_POINT ( 'NONE', #9872 ) ;
#10141 = DIRECTION ( 'NONE',  ( -1.000000000000000000, -0.000000000000000000, -0.000000000000000000 ) ) ;
#10142 = DIRECTION ( 'NONE',  ( -0.9914448613738104932, -0.1305261922200517399, 0.000000000000000000 ) ) ;
#10143 = LINE ( 'NONE', #5580, #5161 ) ;
#10144 = VERTEX_POINT ( 'NONE', #14433 ) ;
#10145 = VERTEX_POINT ( 'NONE', #8354 ) ;
#10146 = FACE_OUTER_BOUND ( 'NONE', #14633, .T. ) ;
#10147 = ORIENTED_EDGE ( 'NONE', *, *, #4100, .F. ) ;
#10148 = VECTOR ( 'NONE', #4796, 1000.000000000000000 ) ;
#10149 = DIRECTION ( 'NONE',  ( 0.000000000000000000, -0.000000000000000000, 1.000000000000000000 ) ) ;
#10150 = CARTESIAN_POINT ( 'NONE',  ( -10.00000000000000000, 0.000000000000000000, 0.000000000000000000 ) ) ;
#10151 = LINE ( 'NONE', #1394, #4193 ) ;
#10152 = EDGE_CURVE ( 'NONE', #6992, #16256, #13022, .T. ) ;
#10153 = ORIENTED_EDGE ( 'NONE', *, *, #4456, .T. ) ;
#10154 = EDGE_CURVE ( 'NONE', #18400, #6, #3982, .T. ) ;
#10155 = CARTESIAN_POINT ( 'NONE',  ( 10.00000000000000000, -13.40641754777683126, 24.79895094899255170 ) ) ;
#10156 = EDGE_CURVE ( 'NONE', #3960, #2157, #11598, .T. ) ;
#10157 = EDGE_LOOP ( 'NONE', ( #6705, #10612, #360, #9533 ) ) ;
#10158 = FACE_BOUND ( 'NONE', #12887, .T. ) ;
#10159 = ORIENTED_EDGE ( 'NONE', *, *, #17962, .F. ) ;
#10160 = ORIENTED_EDGE ( 'NONE', *, *, #9443, .F. ) ;
#10161 = STYLED_ITEM ( 'NONE', ( #8596 ), #13098 ) ;
#10162 = EDGE_CURVE ( 'NONE', #11921, #2367, #6928, .T. ) ;
#10163 = CARTESIAN_POINT ( 'NONE',  ( 0.2500000000000002220, 5.204748896376250699E-16, -4.250000000000000000 ) ) ;
#10164 = DIRECTION ( 'NONE',  ( 0.000000000000000000, 0.000000000000000000, 1.000000000000000000 ) ) ;
#10165 = VERTEX_POINT ( 'NONE', #4074 ) ;
#10166 = VERTEX_POINT ( 'NONE', #6535 ) ;
#10167 = CARTESIAN_POINT ( 'NONE',  ( -79.64793068852898728, -34.99999999999999289, -31.86039329588756530 ) ) ;
#10168 = EDGE_LOOP ( 'NONE', ( #1369, #7298, #9646, #9747 ) ) ;
#10169 = CYLINDRICAL_SURFACE ( 'NONE', #6975, 56.24900000005625600 ) ;
#10170 = EDGE_CURVE ( 'NONE', #944, #17607, #10669, .T. ) ;
#10171 =( GEOMETRIC_REPRESENTATION_CONTEXT ( 3 ) GLOBAL_UNCERTAINTY_ASSIGNED_CONTEXT ( ( #6905 ) ) GLOBAL_UNIT_ASSIGNED_CONTEXT ( ( #2929, #1511, #1782 ) ) REPRESENTATION_CONTEXT ( 'NONE', 'WORKASPACE' ) );
#10172 = DIRECTION ( 'NONE',  ( 0.000000000000000000, 0.000000000000000000, 1.000000000000000000 ) ) ;
#10173 = EDGE_LOOP ( 'NONE', ( #13224, #6197, #8460, #12443 ) ) ;
#10174 = EDGE_CURVE ( 'NONE', #4891, #14252, #8849, .T. ) ;
#10175 = EDGE_CURVE ( 'NONE', #6237, #2958, #5505, .T. ) ;
#10176 = EDGE_LOOP ( 'NONE', ( #16690, #11540, #3256, #10236 ) ) ;
#10177 = DIRECTION ( 'NONE',  ( -1.000000000000000000, 0.000000000000000000, -0.000000000000000000 ) ) ;
#10178 = CARTESIAN_POINT ( 'NONE',  ( 10.00000000000000000, -10.11537145609335830, -55.33199130079796646 ) ) ;
#10179 = DIRECTION ( 'NONE',  ( 0.000000000000000000, -0.7071067811865389130, -0.7071067811865561215 ) ) ;
#10180 = CARTESIAN_POINT ( 'NONE',  ( 0.000000000000000000, 40.19788616105610402, 48.50907078259395888 ) ) ;
#10181 = CARTESIAN_POINT ( 'NONE',  ( -4.197312064133472020, -0.8182229787990021874, -3.502518405183886685 ) ) ;
#10182 = DIRECTION ( 'NONE',  ( 0.000000000000000000, 0.000000000000000000, 1.000000000000000000 ) ) ;
#10183 = DIRECTION ( 'NONE',  ( -1.000000000000000000, -0.000000000000000000, 0.000000000000000000 ) ) ;
#10184 = DIRECTION ( 'NONE',  ( 1.000000000000000000, 0.000000000000000000, 0.000000000000000000 ) ) ;
#10185 = VERTEX_POINT ( 'NONE', #7102 ) ;
#10186 = DIRECTION ( 'NONE',  ( -1.000000000000000000, -0.000000000000000000, -0.000000000000000000 ) ) ;
#10187 = EDGE_CURVE ( 'NONE', #1965, #13213, #5784, .T. ) ;
#10188 = DIRECTION ( 'NONE',  ( -1.000000000000000000, 0.000000000000000000, 0.000000000000000000 ) ) ;
#10189 = AXIS2_PLACEMENT_3D ( 'NONE', #16331, #3287, #8984 ) ;
#10190 = ORIENTED_EDGE ( 'NONE', *, *, #4704, .F. ) ;
#10191 = DIRECTION ( 'NONE',  ( -0.000000000000000000, 1.000000000000000000, -0.000000000000000000 ) ) ;
#10192 = CARTESIAN_POINT ( 'NONE',  ( 0.000000000000000000, 1.489278925039883239, -26.20671763660627107 ) ) ;
#10193 = CIRCLE ( 'NONE', #8061, 33.00000000003299760 ) ;
#10194 = AXIS2_PLACEMENT_3D ( 'NONE', #15312, #6369, #9588 ) ;
#10195 = ORIENTED_EDGE ( 'NONE', *, *, #9136, .T. ) ;
#10196 = CARTESIAN_POINT ( 'NONE',  ( -3.098410542199071749, -7.060458129626440815, -1.000000000000000000 ) ) ;
#10197 = PLANE ( 'NONE',  #4453 ) ;
#10198 = AXIS2_PLACEMENT_3D ( 'NONE', #10702, #13672, #2226 ) ;
#10199 = DIRECTION ( 'NONE',  ( -1.000000000000000000, -0.000000000000000000, -0.000000000000000000 ) ) ;
#10200 = AXIS2_PLACEMENT_3D ( 'NONE', #15681, #1218, #8538 ) ;
#10201 = ORIENTED_EDGE ( 'NONE', *, *, #496, .T. ) ;
#10202 = CARTESIAN_POINT ( 'NONE',  ( 0.000000000000000000, -13.75000000000000533, 0.000000000000000000 ) ) ;
#10203 = DIRECTION ( 'NONE',  ( 0.000000000000000000, 0.9876883405951371042, 0.1564344650402347547 ) ) ;
#10204 = FACE_OUTER_BOUND ( 'NONE', #17983, .T. ) ;
#10205 = DIRECTION ( 'NONE',  ( -1.000000000000000000, 0.000000000000000000, 0.000000000000000000 ) ) ;
#10206 = CARTESIAN_POINT ( 'NONE',  ( 0.000000000000000000, -48.50907078259351835, -40.19788616105663692 ) ) ;
#10207 = ORIENTED_EDGE ( 'NONE', *, *, #10985, .F. ) ;
#10208 = DIRECTION ( 'NONE',  ( 0.000000000000000000, 0.000000000000000000, 1.000000000000000000 ) ) ;
#10209 = ORIENTED_EDGE ( 'NONE', *, *, #2615, .F. ) ;
#10210 = EDGE_CURVE ( 'NONE', #7394, #7573, #3070, .T. ) ;
#10211 = DIRECTION ( 'NONE',  ( -0.000000000000000000, 0.000000000000000000, 1.000000000000000000 ) ) ;
#10212 = DIRECTION ( 'NONE',  ( -0.000000000000000000, 1.000000000000000000, -0.000000000000000000 ) ) ;
#10213 = EDGE_LOOP ( 'NONE', ( #13254, #15672, #3222, #2310 ) ) ;
#10214 = CIRCLE ( 'NONE', #1991, 2.649999999999992806 ) ;
#10215 = CIRCLE ( 'NONE', #490, 56.24900000005626310 ) ;
#10216 = APPLICATION_PROTOCOL_DEFINITION ( 'draft international standard', 'automotive_design', 1998, #10116 ) ;
#10217 = ORIENTED_EDGE ( 'NONE', *, *, #10960, .F. ) ;
#10218 = CIRCLE ( 'NONE', #16926, 24.00000000002399858 ) ;
#10219 = AXIS2_PLACEMENT_3D ( 'NONE', #13917, #2194, #18197 ) ;
#10220 = EDGE_CURVE ( 'NONE', #3486, #9332, #3694, .T. ) ;
#10221 = PLANE ( 'NONE',  #8993 ) ;
#10222 = DIRECTION ( 'NONE',  ( 0.000000000000000000, 0.000000000000000000, 1.000000000000000000 ) ) ;
#10223 = CARTESIAN_POINT ( 'NONE',  ( -11.25000000000000533, 0.000000000000000000, 0.000000000000000000 ) ) ;
#10224 = CARTESIAN_POINT ( 'NONE',  ( 10.00000000000000000, 0.000000000000000000, 0.000000000000000000 ) ) ;
#10225 = ADVANCED_FACE ( 'NONE', ( #7299 ), #14161, .T. ) ;
#10226 = AXIS2_PLACEMENT_3D ( 'NONE', #4493, #10388, #14587 ) ;
#10227 = CARTESIAN_POINT ( 'NONE',  ( 10.00000000000000000, -20.41355805489629915, 19.44239304137368407 ) ) ;
#10228 = DIRECTION ( 'NONE',  ( 0.000000000000000000, 1.000000000000000000, 3.469446951950144779E-15 ) ) ;
#10229 = CIRCLE ( 'NONE', #15106, 24.00000000002399858 ) ;
#10230 = LINE ( 'NONE', #9857, #873 ) ;
#10231 = VECTOR ( 'NONE', #661, 1000.000000000000000 ) ;
#10232 = ORIENTED_EDGE ( 'NONE', *, *, #2383, .F. ) ;
#10233 = FACE_OUTER_BOUND ( 'NONE', #9862, .T. ) ;
#10234 = DIRECTION ( 'NONE',  ( 0.000000000000000000, 0.000000000000000000, -1.000000000000000000 ) ) ;
#10235 = DIRECTION ( 'NONE',  ( 0.000000000000000000, 0.000000000000000000, 1.000000000000000000 ) ) ;
#10236 = ORIENTED_EDGE ( 'NONE', *, *, #11031, .T. ) ;
#10237 = VERTEX_POINT ( 'NONE', #2739 ) ;
#10238 = LINE ( 'NONE', #4161, #180 ) ;
#10239 = SURFACE_STYLE_FILL_AREA ( #3103 ) ;
#10240 = VERTEX_POINT ( 'NONE', #8542 ) ;
#10241 = AXIS2_PLACEMENT_3D ( 'NONE', #17423, #1154, #18663 ) ;
#10242 = AXIS2_PLACEMENT_3D ( 'NONE', #8757, #4209, #10377 ) ;
#10243 = AXIS2_PLACEMENT_3D ( 'NONE', #14005, #17152, #18375 ) ;
#10244 = CIRCLE ( 'NONE', #8717, 8.099999999999999645 ) ;
#10245 = DIRECTION ( 'NONE',  ( -0.000000000000000000, 1.000000000000000000, -0.000000000000000000 ) ) ;
#10246 = DIRECTION ( 'NONE',  ( -0.7071067811865254793, 8.659560562355202797E-17, -0.7071067811865695552 ) ) ;
#10247 = LINE ( 'NONE', #14719, #18472 ) ;
#10248 = ORIENTED_EDGE ( 'NONE', *, *, #3129, .F. ) ;
#10249 = DIRECTION ( 'NONE',  ( 0.000000000000000000, 0.000000000000000000, -1.000000000000000000 ) ) ;
#10250 = CIRCLE ( 'NONE', #9960, 63.00000000006298961 ) ;
#10251 = ORIENTED_EDGE ( 'NONE', *, *, #4251, .T. ) ;
#10252 = DIRECTION ( 'NONE',  ( 1.000000000000000000, 0.000000000000000000, 0.000000000000000000 ) ) ;
#10253 = VERTEX_POINT ( 'NONE', #14350 ) ;
#10254 = VERTEX_POINT ( 'NONE', #1313 ) ;
#10255 = CIRCLE ( 'NONE', #17801, 24.00000000002399858 ) ;
#10256 = CYLINDRICAL_SURFACE ( 'NONE', #16097, 56.24900000005625600 ) ;
#10257 = DIRECTION ( 'NONE',  ( 0.000000000000000000, 0.000000000000000000, -1.000000000000000000 ) ) ;
#10258 = AXIS2_PLACEMENT_3D ( 'NONE', #5685, #7386, #13116 ) ;
#10259 = ORIENTED_EDGE ( 'NONE', *, *, #6714, .F. ) ;
#10260 = ORIENTED_EDGE ( 'NONE', *, *, #9868, .F. ) ;
#10261 = CIRCLE ( 'NONE', #12701, 2.649999999999999467 ) ;
#10262 = LINE ( 'NONE', #1323, #8079 ) ;
#10263 = ORIENTED_EDGE ( 'NONE', *, *, #14704, .F. ) ;
#10264 = CARTESIAN_POINT ( 'NONE',  ( 0.000000000000000000, -34.99999999999999289, 0.000000000000000000 ) ) ;
#10265 = EDGE_CURVE ( 'NONE', #11258, #16371, #12818, .T. ) ;
#10266 = EDGE_CURVE ( 'NONE', #18700, #14293, #14950, .T. ) ;
#10267 = CIRCLE ( 'NONE', #15452, 56.24900000005624889 ) ;
#10268 = AXIS2_PLACEMENT_3D ( 'NONE', #3185, #333, #9084 ) ;
#10269 = DIRECTION ( 'NONE',  ( 0.000000000000000000, 0.000000000000000000, 1.000000000000000000 ) ) ;
#10270 = AXIS2_PLACEMENT_3D ( 'NONE', #5590, #11774, #17583 ) ;
#10271 = VECTOR ( 'NONE', #4314, 1000.000000000000000 ) ;
#10272 = VERTEX_POINT ( 'NONE', #7389 ) ;
#10273 = PRODUCT_DEFINITION_SHAPE ( 'NONE', 'NONE',  #18839 ) ;
#10274 = ORIENTED_EDGE ( 'NONE', *, *, #5342, .T. ) ;
#10275 = DIRECTION ( 'NONE',  ( 0.000000000000000000, 0.000000000000000000, 1.000000000000000000 ) ) ;
#10276 = CYLINDRICAL_SURFACE ( 'NONE', #1971, 150.0000000000000284 ) ;
#10277 = CARTESIAN_POINT ( 'NONE',  ( 0.000000000000000000, -1.178949249685218748, -2.041999999999998039 ) ) ;
#10278 = ORIENTED_EDGE ( 'NONE', *, *, #12828, .T. ) ;
#10279 = CARTESIAN_POINT ( 'NONE',  ( 10.00000000000000000, 24.68609584167230153, -50.69000562871616467 ) ) ;
#10280 = EDGE_CURVE ( 'NONE', #1567, #11247, #6146, .T. ) ;
#10281 = DIRECTION ( 'NONE',  ( 0.000000000000000000, -1.000000000000000000, 0.000000000000000000 ) ) ;
#10282 = DIRECTION ( 'NONE',  ( 1.000000000000000000, -0.000000000000000000, -0.000000000000000000 ) ) ;
#10283 = CIRCLE ( 'NONE', #12718, 12.00000000001200640 ) ;
#10284 = FACE_BOUND ( 'NONE', #2404, .T. ) ;
#10285 = EDGE_LOOP ( 'NONE', ( #10121, #11645, #14908 ) ) ;
#10286 = DIRECTION ( 'NONE',  ( 0.000000000000000000, 0.8090169943749486725, -0.5877852522924714718 ) ) ;
#10287 = CIRCLE ( 'NONE', #6021, 63.00000000006298961 ) ;
#10288 = ORIENTED_EDGE ( 'NONE', *, *, #6913, .T. ) ;
#10289 = DIRECTION ( 'NONE',  ( -1.000000000000000000, -0.000000000000000000, -0.000000000000000000 ) ) ;
#10290 = FACE_OUTER_BOUND ( 'NONE', #13169, .T. ) ;
#10291 = CIRCLE ( 'NONE', #4497, 4.250000000000000000 ) ;
#10292 = AXIS2_PLACEMENT_3D ( 'NONE', #15993, #3050, #9901 ) ;
#10293 = EDGE_CURVE ( 'NONE', #11990, #17080, #5204, .T. ) ;
#10294 = EDGE_CURVE ( 'NONE', #7932, #15825, #8818, .T. ) ;
#10295 = EDGE_CURVE ( 'NONE', #17597, #475, #7636, .T. ) ;
#10296 = AXIS2_PLACEMENT_3D ( 'NONE', #16889, #5358, #12411 ) ;
#10297 = EDGE_CURVE ( 'NONE', #3888, #7917, #433, .T. ) ;
#10298 = EDGE_LOOP ( 'NONE', ( #5048, #15406, #1322, #2926 ) ) ;
#10299 = AXIS2_PLACEMENT_3D ( 'NONE', #10938, #15324, #3430 ) ;
#10300 = DIRECTION ( 'NONE',  ( 1.000000000000000000, 0.000000000000000000, 0.000000000000000000 ) ) ;
#10301 = DIRECTION ( 'NONE',  ( -1.000000000000000000, 0.000000000000000000, 0.000000000000000000 ) ) ;
#10302=STYLED_ITEM('',(#18890),#15847);
#10303 = ORIENTED_EDGE ( 'NONE', *, *, #18202, .F. ) ;
#10304 = CIRCLE ( 'NONE', #14555, 56.24900000005624889 ) ;
#10305 = CYLINDRICAL_SURFACE ( 'NONE', #579, 30.00000000000000000 ) ;
#10306 = DIRECTION ( 'NONE',  ( 0.1305261922200524616, -0.9914448613738103822, 0.000000000000000000 ) ) ;
#10307 = ADVANCED_FACE ( 'NONE', ( #11957 ), #8909, .T. ) ;
#10308 = CARTESIAN_POINT ( 'NONE',  ( 10.00000000000000000, 16.10733642026482570, 53.89344778774818678 ) ) ;
#10309 = CARTESIAN_POINT ( 'NONE',  ( 0.000000000000000000, -55.74967257055887870, 7.478235706488783663 ) ) ;
#10310 = CARTESIAN_POINT ( 'NONE',  ( 4.999999999999999112, -15.61693798565454472, -61.03368945066451801 ) ) ;
#10311 = ORIENTED_EDGE ( 'NONE', *, *, #4005, .F. ) ;
#10312 = FACE_OUTER_BOUND ( 'NONE', #8869, .T. ) ;
#10313 = ORIENTED_EDGE ( 'NONE', *, *, #5959, .T. ) ;
#10314 =( NAMED_UNIT ( * ) SI_UNIT ( $, .STERADIAN. ) SOLID_ANGLE_UNIT ( ) );
#10315 = DIRECTION ( 'NONE',  ( 0.000000000000000000, 0.000000000000000000, 1.000000000000000000 ) ) ;
#10316 = AXIS2_PLACEMENT_3D ( 'NONE', #16210, #8954, #1724 ) ;
#10317 = ORIENTED_EDGE ( 'NONE', *, *, #15860, .F. ) ;
#10318 = APPLICATION_PROTOCOL_DEFINITION ( 'draft international standard', 'automotive_design', 1998, #2938 ) ;
#10319 = AXIS2_PLACEMENT_3D ( 'NONE', #6469, #9316, #4943 ) ;
#10320 = ORIENTED_EDGE ( 'NONE', *, *, #12451, .F. ) ;
#10321 = ADVANCED_FACE ( 'NONE', ( #15013 ), #9101, .T. ) ;
#10322 = CARTESIAN_POINT ( 'NONE',  ( 10.00000000000000000, 0.000000000000000000, 0.000000000000000000 ) ) ;
#10323 = CYLINDRICAL_SURFACE ( 'NONE', #13111, 26.24900000002624978 ) ;
#10324 = CIRCLE ( 'NONE', #11842, 2.649999999999995914 ) ;
#10325 = DIRECTION ( 'NONE',  ( -1.000000000000000000, -0.000000000000000000, -0.000000000000000000 ) ) ;
#10326 = CARTESIAN_POINT ( 'NONE',  ( 0.000000000000000000, 3.000000000000000000, -55.00000000000000000 ) ) ;
#10327 = CIRCLE ( 'NONE', #1813, 2.700000000000000622 ) ;
#10328 = DIRECTION ( 'NONE',  ( -1.000000000000000000, 0.000000000000000000, 0.000000000000000000 ) ) ;
#10329 = CARTESIAN_POINT ( 'NONE',  ( 10.00000000000000178, 6.799999999999999822, -1.500000000000000000 ) ) ;
#10330 = CYLINDRICAL_SURFACE ( 'NONE', #6954, 4.250000000000000000 ) ;
#10331 = ORIENTED_EDGE ( 'NONE', *, *, #15364, .F. ) ;
#10332 = DIRECTION ( 'NONE',  ( -1.000000000000000000, -0.000000000000000000, 0.000000000000000000 ) ) ;
#10333 = CARTESIAN_POINT ( 'NONE',  ( 0.000000000000000000, -26.50000000000000000, 0.000000000000000000 ) ) ;
#10334 = CARTESIAN_POINT ( 'NONE',  ( 2.500000000000000000, 0.000000000000000000, 0.000000000000000000 ) ) ;
#10335 = EDGE_LOOP ( 'NONE', ( #18611, #17533, #15083, #8333 ) ) ;
#10336 = ORIENTED_EDGE ( 'NONE', *, *, #1793, .F. ) ;
#10337 = DIRECTION ( 'NONE',  ( 0.000000000000000000, -0.4539904997395542430, 0.8910065241883641241 ) ) ;
#10338 = CARTESIAN_POINT ( 'NONE',  ( 0.000000000000000000, 61.03368945066456774, -15.61693798565434399 ) ) ;
#10339 = EDGE_LOOP ( 'NONE', ( #18150, #11738, #7912, #222 ) ) ;
#10340 = AXIS2_PLACEMENT_3D ( 'NONE', #16048, #13190, #15950 ) ;
#10341 = CIRCLE ( 'NONE', #4869, 0.2000000000000000944 ) ;
#10342 = EDGE_CURVE ( 'NONE', #13575, #10719, #15861, .T. ) ;
#10343 = FACE_OUTER_BOUND ( 'NONE', #2628, .T. ) ;
#10344 = CARTESIAN_POINT ( 'NONE',  ( 0.5276280594147412240, -4.314175951381924889, -3.320322319201654881 ) ) ;
#10345 = DIRECTION ( 'NONE',  ( 0.000000000000000000, 0.3090169943749480619, -0.9510565162951533091 ) ) ;
#10346 = ORIENTED_EDGE ( 'NONE', *, *, #7272, .F. ) ;
#10347 = DIRECTION ( 'NONE',  ( 1.000000000000000000, 0.000000000000000000, 0.000000000000000000 ) ) ;
#10348 = ORIENTED_EDGE ( 'NONE', *, *, #9224, .F. ) ;
#10349 = AXIS2_PLACEMENT_3D ( 'NONE', #16314, #9075, #7643 ) ;
#10350 = DIRECTION ( 'NONE',  ( 0.000000000000000000, 0.000000000000000000, 1.000000000000000000 ) ) ;
#10351 = ORIENTED_EDGE ( 'NONE', *, *, #16811, .F. ) ;
#10352 = CARTESIAN_POINT ( 'NONE',  ( -117.1020693116508085, -30.00000000000000000, 19.69080595179778115 ) ) ;
#10353 = CARTESIAN_POINT ( 'NONE',  ( -6.473970235329672780E-16, -4.862606272033106691, -3.745885042887442395 ) ) ;
#10354 = ORIENTED_EDGE ( 'NONE', *, *, #18370, .T. ) ;
#10355 = ORIENTED_EDGE ( 'NONE', *, *, #1172, .F. ) ;
#10356 = EDGE_CURVE ( 'NONE', #205, #4486, #14336, .T. ) ;
#10357 = DIRECTION ( 'NONE',  ( -1.000000000000000000, 0.000000000000000000, 0.000000000000000000 ) ) ;
#10358 = ORIENTED_EDGE ( 'NONE', *, *, #7087, .T. ) ;
#10359 = DIRECTION ( 'NONE',  ( -0.000000000000000000, 1.000000000000000000, -0.000000000000000000 ) ) ;
#10360 = EDGE_CURVE ( 'NONE', #14252, #13512, #9003, .T. ) ;
#10361 =( REPRESENTATION_RELATIONSHIP ('NONE','NONE', #11014, #13460 ) REPRESENTATION_RELATIONSHIP_WITH_TRANSFORMATION ( #7819 )SHAPE_REPRESENTATION_RELATIONSHIP( ) );
#10362 = CIRCLE ( 'NONE', #4001, 24.00000000002399858 ) ;
#10363 = CARTESIAN_POINT ( 'NONE',  ( 10.00000000000000000, 54.20017844242556748, -32.11449294037137747 ) ) ;
#10364 = VERTEX_POINT ( 'NONE', #17585 ) ;
#10365 = EDGE_LOOP ( 'NONE', ( #4593, #11998, #3032, #7919, #10766, #11927 ) ) ;
#10366 = CARTESIAN_POINT ( 'NONE',  ( 10.00000000000000000, 0.000000000000000000, 0.000000000000000000 ) ) ;
#10367 = DIRECTION ( 'NONE',  ( 1.000000000000000000, 0.000000000000000000, 0.000000000000000000 ) ) ;
#10368 = DIRECTION ( 'NONE',  ( 0.000000000000000000, -1.000000000000000000, -0.000000000000000000 ) ) ;
#10369 = ORIENTED_EDGE ( 'NONE', *, *, #4093, .F. ) ;
#10370 = CARTESIAN_POINT ( 'NONE',  ( 2.500000000000000000, 1.178949249685218081, 2.041999999999998483 ) ) ;
#10371 = CARTESIAN_POINT ( 'NONE',  ( 2.171643655288379993, -3.365003104552334978, -1.195831703456429434E-14 ) ) ;
#10372 = CARTESIAN_POINT ( 'NONE',  ( 0.000000000000000000, -14.27431201565546637, 29.75305054077467304 ) ) ;
#10373 = LINE ( 'NONE', #15997, #2318 ) ;
#10374 = VERTEX_POINT ( 'NONE', #1862 ) ;
#10375 = CARTESIAN_POINT ( 'NONE',  ( 10.00000000000000000, -62.72529079327811274, 5.876895005582225551 ) ) ;
#10376 = AXIS2_PLACEMENT_3D ( 'NONE', #15857, #2806, #13004 ) ;
#10377 = DIRECTION ( 'NONE',  ( 0.000000000000000000, 0.000000000000000000, -1.000000000000000000 ) ) ;
#10378 = ORIENTED_EDGE ( 'NONE', *, *, #9250, .T. ) ;
#10379 = DIRECTION ( 'NONE',  ( -1.000000000000000000, 0.000000000000000000, 0.000000000000000000 ) ) ;
#10380 = CARTESIAN_POINT ( 'NONE',  ( -290.0000000000001137, -30.00000000000000000, -125.0000000000000000 ) ) ;
#10381 = VERTEX_POINT ( 'NONE', #14919 ) ;
#10382 = AXIS2_PLACEMENT_3D ( 'NONE', #1008, #6808, #6903 ) ;
#10383 = FACE_OUTER_BOUND ( 'NONE', #13524, .T. ) ;
#10384 = LINE ( 'NONE', #13245, #10953 ) ;
#10385 = ORIENTED_EDGE ( 'NONE', *, *, #2865, .T. ) ;
#10386 = FACE_OUTER_BOUND ( 'NONE', #9012, .T. ) ;
#10387 = ADVANCED_FACE ( 'NONE', ( #5871, #16158 ), #3112, .T. ) ;
#10388 = DIRECTION ( 'NONE',  ( 0.000000000000000000, 1.000000000000000000, 0.000000000000000000 ) ) ;
#10389 = EDGE_CURVE ( 'NONE', #6043, #16740, #11297, .T. ) ;
#10390 = CIRCLE ( 'NONE', #18300, 26.24900000002624978 ) ;
#10391 = EDGE_CURVE ( 'NONE', #16921, #15596, #12425, .T. ) ;
#10392 = CIRCLE ( 'NONE', #16174, 2.649999999999995914 ) ;
#10393 = CARTESIAN_POINT ( 'NONE',  ( -10.00000000000000000, 0.000000000000000000, 0.000000000000000000 ) ) ;
#10394 = CYLINDRICAL_SURFACE ( 'NONE', #2183, 24.00000000002400213 ) ;
#10395 = DIRECTION ( 'NONE',  ( -0.000000000000000000, 1.000000000000000000, -0.000000000000000000 ) ) ;
#10396 = ORIENTED_EDGE ( 'NONE', *, *, #11595, .F. ) ;
#10397 = CARTESIAN_POINT ( 'NONE',  ( 10.00000000000000000, -27.94286728106390072, -3.730438010304629515 ) ) ;
#10398 = ORIENTED_EDGE ( 'NONE', *, *, #18307, .T. ) ;
#10399 = EDGE_CURVE ( 'NONE', #195, #18379, #6117, .T. ) ;
#10400 = FACE_OUTER_BOUND ( 'NONE', #1133, .T. ) ;
#10401 = ORIENTED_EDGE ( 'NONE', *, *, #12237, .F. ) ;
#10402 = ITEM_DEFINED_TRANSFORMATION ( 'NONE', 'NONE', #2273,  #8017 ) ;
#10403 = ORIENTED_EDGE ( 'NONE', *, *, #15326, .F. ) ;
#10404 = VERTEX_POINT ( 'NONE', #13850 ) ;
#10405 = EDGE_CURVE ( 'NONE', #14912, #9886, #17098, .T. ) ;
#10406 = EDGE_LOOP ( 'NONE', ( #8565, #3474, #6118, #13719 ) ) ;
#10407 = DIRECTION ( 'NONE',  ( -0.000000000000000000, 1.000000000000000000, -0.000000000000000000 ) ) ;
#10408 = DIRECTION ( 'NONE',  ( -1.000000000000000000, 0.000000000000000000, 0.000000000000000000 ) ) ;
#10409 = CARTESIAN_POINT ( 'NONE',  ( -10.00000000000000000, 0.000000000000000000, 0.000000000000000000 ) ) ;
#10410 = DIRECTION ( 'NONE',  ( 0.000000000000000000, 0.000000000000000000, 1.000000000000000000 ) ) ;
#10411 = ADVANCED_FACE ( 'NONE', ( #8147 ), #11080, .T. ) ;
#10412 = CARTESIAN_POINT ( 'NONE',  ( 0.000000000000000000, -27.72801475327278453, 6.913036516934497833 ) ) ;
#10413 = DIRECTION ( 'NONE',  ( 0.000000000000000000, 0.8090169943749446757, 0.5877852522924769119 ) ) ;
#10414 = FACE_OUTER_BOUND ( 'NONE', #18053, .T. ) ;
#10415 = DIRECTION ( 'NONE',  ( 1.000000000000000000, 0.000000000000000000, 0.000000000000000000 ) ) ;
#10416 = VERTEX_POINT ( 'NONE', #3587 ) ;
#10417 = AXIS2_PLACEMENT_3D ( 'NONE', #8915, #5878, #1320 ) ;
#10418 = DIRECTION ( 'NONE',  ( 0.9938152567191714803, 0.000000000000000000, -0.1110460963393456596 ) ) ;
#10419 = CARTESIAN_POINT ( 'NONE',  ( 0.000000000000000000, 0.000000000000000000, 0.000000000000000000 ) ) ;
#10420 = CARTESIAN_POINT ( 'NONE',  ( 21.00000000000000355, 2.516649172247811061E-16, -2.055000000000000160 ) ) ;
#10421 = ORIENTED_EDGE ( 'NONE', *, *, #14588, .F. ) ;
#10422 = ORIENTED_EDGE ( 'NONE', *, *, #10389, .F. ) ;
#10423 = EDGE_CURVE ( 'NONE', #2818, #104, #18324, .T. ) ;
#10424 = DIRECTION ( 'NONE',  ( -1.000000000000000000, -0.000000000000000000, 0.000000000000000000 ) ) ;
#10425 = DIRECTION ( 'NONE',  ( -1.000000000000000000, -0.000000000000000000, -0.000000000000000000 ) ) ;
#10426 = VERTEX_POINT ( 'NONE', #12432 ) ;
#10427 = VECTOR ( 'NONE', #2438, 1000.000000000000000 ) ;
#10428 = CARTESIAN_POINT ( 'NONE',  ( -2.000000000000007550, -3.464101615137749945, 0.000000000000000000 ) ) ;
#10429 = DIRECTION ( 'NONE',  ( -1.000000000000000000, -0.000000000000000000, 0.000000000000000000 ) ) ;
#10430 = DIRECTION ( 'NONE',  ( 0.000000000000000000, 0.000000000000000000, 1.000000000000000000 ) ) ;
#10431 = EDGE_LOOP ( 'NONE', ( #7757, #4278, #9716, #11586 ) ) ;
#10432 = CARTESIAN_POINT ( 'NONE',  ( 0.000000000000000000, 13.40641754777700534, -24.79895094899245933 ) ) ;
#10433 = EDGE_LOOP ( 'NONE', ( #7579, #1941, #4506, #12197 ) ) ;
#10434 = CARTESIAN_POINT ( 'NONE',  ( 10.00000000000000000, -32.11449294037157642, -54.20017844242546090 ) ) ;
#10435 = ORIENTED_EDGE ( 'NONE', *, *, #12638, .F. ) ;
#10436 = FACE_OUTER_BOUND ( 'NONE', #13593, .T. ) ;
#10437 = CARTESIAN_POINT ( 'NONE',  ( -117.1020693116506379, -38.00000000000000000, -19.69080595179801207 ) ) ;
#10438 = ORIENTED_EDGE ( 'NONE', *, *, #1807, .T. ) ;
#10439 = ORIENTED_EDGE ( 'NONE', *, *, #14622, .T. ) ;
#10440 = ADVANCED_FACE ( 'NONE', ( #3862 ), #2233, .T. ) ;
#10441 = CARTESIAN_POINT ( 'NONE',  ( 10.00000000000000000, -29.03656532225574693, 15.68049343255986017 ) ) ;
#10442 = AXIS2_PLACEMENT_3D ( 'NONE', #18314, #8025, #6795 ) ;
#10443 = ORIENTED_EDGE ( 'NONE', *, *, #9720, .F. ) ;
#10444 = CARTESIAN_POINT ( 'NONE',  ( 0.000000000000000000, 53.92768374110868734, 16.45250512421953459 ) ) ;
#10445 = CARTESIAN_POINT ( 'NONE',  ( 2.725741868436127202, -3.045094352033990148, -3.220599429844051453 ) ) ;
#10446 = EDGE_LOOP ( 'NONE', ( #11875, #1676 ) ) ;
#10447 = EDGE_CURVE ( 'NONE', #12652, #645, #9476, .T. ) ;
#10448 = VERTEX_POINT ( 'NONE', #5093 ) ;
#10449 = DIRECTION ( 'NONE',  ( 1.000000000000000000, 0.000000000000000000, 0.000000000000000000 ) ) ;
#10450 = CYLINDRICAL_SURFACE ( 'NONE', #2575, 12.00000000001200107 ) ;
#10451 = DIRECTION ( 'NONE',  ( 0.000000000000000000, 0.000000000000000000, 1.000000000000000000 ) ) ;
#10452 = ORIENTED_EDGE ( 'NONE', *, *, #2482, .T. ) ;
#10453 = DIRECTION ( 'NONE',  ( 0.000000000000000000, 0.000000000000000000, 1.000000000000000000 ) ) ;
#10454 = EDGE_CURVE ( 'NONE', #10381, #18246, #8561, .T. ) ;
#10455 = DIRECTION ( 'NONE',  ( -1.000000000000000000, -0.000000000000000000, 0.000000000000000000 ) ) ;
#10456 = DIRECTION ( 'NONE',  ( -1.000000000000000000, 0.000000000000000000, 0.000000000000000000 ) ) ;
#10457 = CARTESIAN_POINT ( 'NONE',  ( 0.000000000000000000, 0.000000000000000000, 0.000000000000000000 ) ) ;
#10458 = ORIENTED_EDGE ( 'NONE', *, *, #5149, .T. ) ;
#10459 = CYLINDRICAL_SURFACE ( 'NONE', #18542, 24.00000000002399503 ) ;
#10460 = VERTEX_POINT ( 'NONE', #9663 ) ;
#10461 = CARTESIAN_POINT ( 'NONE',  ( 2.500000000000000000, 1.178949249685213863, -2.042000000000001148 ) ) ;
#10462 = CYLINDRICAL_SURFACE ( 'NONE', #404, 24.00000000002399503 ) ;
#10463 = APPLICATION_CONTEXT ( 'automotive_design' ) ;
#10464 = PRESENTATION_LAYER_ASSIGNMENT (  '', '', ( #18688 ) ) ;
#10465 = ORIENTED_EDGE ( 'NONE', *, *, #5157, .T. ) ;
#10466 = CYLINDRICAL_SURFACE ( 'NONE', #9644, 8.099999999999999645 ) ;
#10467 = CARTESIAN_POINT ( 'NONE',  ( 13.90576474687299680, 10.00000000000000000, 45.44754323328179169 ) ) ;
#10468 = ORIENTED_EDGE ( 'NONE', *, *, #3196, .F. ) ;
#10469 =( NAMED_UNIT ( * ) SI_UNIT ( $, .STERADIAN. ) SOLID_ANGLE_UNIT ( ) );
#10470 = DIRECTION ( 'NONE',  ( 0.000000000000000000, -1.000000000000000000, 0.000000000000000000 ) ) ;
#10471 = AXIS2_PLACEMENT_3D ( 'NONE', #7940, #6512, #1756 ) ;
#10472 = CYLINDRICAL_SURFACE ( 'NONE', #885, 24.00000000002399858 ) ;
#10473 = DIRECTION ( 'NONE',  ( -1.000000000000000000, -0.000000000000000000, -0.000000000000000000 ) ) ;
#10474 = DIRECTION ( 'NONE',  ( 0.000000000000000000, 0.000000000000000000, 1.000000000000000000 ) ) ;
#10475 = VERTEX_POINT ( 'NONE', #12235 ) ;
#10476 = CYLINDRICAL_SURFACE ( 'NONE', #590, 56.24900000005625600 ) ;
#10477 = VERTEX_POINT ( 'NONE', #18142 ) ;
#10478 = B_SPLINE_CURVE_WITH_KNOTS ( 'NONE', 3,
 ( #8888, #12023, #17662, #1935, #4892 ),
 .UNSPECIFIED., .F., .F.,
 ( 4, 1, 4 ),
 ( 5.640274452250024914E-20, 0.002309401076758505356, 0.004618802153517010713 ),
 .UNSPECIFIED. ) ;
#10479 = VECTOR ( 'NONE', #14941, 1000.000000000000000 ) ;
#10480 = CARTESIAN_POINT ( 'NONE',  ( 50.00005079999999680, 0.000000000000000000, 1.500000000000000000 ) ) ;
#10481 = EDGE_LOOP ( 'NONE', ( #766, #3900, #11914, #16255 ) ) ;
#10482 = ITEM_DEFINED_TRANSFORMATION ( 'NONE', 'NONE', #16877,  #8017 ) ;
#10483 = ORIENTED_EDGE ( 'NONE', *, *, #15399, .T. ) ;
#10484 = EDGE_CURVE ( 'NONE', #12824, #17009, #1267, .T. ) ;
#10485 = PRODUCT_DEFINITION_FORMATION_WITH_SPECIFIED_SOURCE ( 'ANY', '', #2666, .NOT_KNOWN. ) ;
#10486 = ADVANCED_FACE ( 'NONE', ( #18243 ), #4910, .T. ) ;
#10487 = EDGE_LOOP ( 'NONE', ( #15753, #1140, #16745, #15516, #10501 ) ) ;
#10488 = CIRCLE ( 'NONE', #14755, 56.24900000005624889 ) ;
#10489 = AXIS2_PLACEMENT_3D ( 'NONE', #10073, #13561, #2832 ) ;
#10490 = ORIENTED_EDGE ( 'NONE', *, *, #13196, .T. ) ;
#10491 = DIRECTION ( 'NONE',  ( 0.000000000000000000, 0.000000000000000000, 1.000000000000000000 ) ) ;
#10492 = ADVANCED_FACE ( 'NONE', ( #536, #18330 ), #4992, .T. ) ;
#10493 = CARTESIAN_POINT ( 'NONE',  ( 0.000000000000000000, 26.49895292618005271, 49.76630880786320432 ) ) ;
#10494 = DIRECTION ( 'NONE',  ( 0.000000000000000000, 0.000000000000000000, 1.000000000000000000 ) ) ;
#10495 = DIRECTION ( 'NONE',  ( 0.000000000000000000, 0.000000000000000000, 1.000000000000000000 ) ) ;
#10496 = ADVANCED_FACE ( 'NONE', ( #10990 ), #4909, .T. ) ;
#10497 = LINE ( 'NONE', #17744, #13610 ) ;
#10498 = CARTESIAN_POINT ( 'NONE',  ( 0.000000000000000000, -17.25000000000000355, 25.00000000000000000 ) ) ;
#10499 = DIRECTION ( 'NONE',  ( 0.000000000000000000, 0.000000000000000000, -1.000000000000000000 ) ) ;
#10500 = DIRECTION ( 'NONE',  ( -1.000000000000000000, 0.000000000000000000, 0.000000000000000000 ) ) ;
#10501 = ORIENTED_EDGE ( 'NONE', *, *, #2238, .T. ) ;
#10502 = CARTESIAN_POINT ( 'NONE',  ( 0.000000000000000000, -17.25000000000000355, 0.000000000000000000 ) ) ;
#10503 = EDGE_CURVE ( 'NONE', #11649, #7339, #10799, .T. ) ;
#10504 = FACE_OUTER_BOUND ( 'NONE', #9299, .T. ) ;
#10505 = CARTESIAN_POINT ( 'NONE',  ( 0.000000000000000000, 0.000000000000000000, 0.000000000000000000 ) ) ;
#10506 = ORIENTED_EDGE ( 'NONE', *, *, #13877, .T. ) ;
#10507 = CIRCLE ( 'NONE', #15977, 12.00000000001200817 ) ;
#10508 = ORIENTED_EDGE ( 'NONE', *, *, #2375, .F. ) ;
#10509 = AXIS2_PLACEMENT_3D ( 'NONE', #13166, #14769, #8952 ) ;
#10510 = DIRECTION ( 'NONE',  ( -1.000000000000000000, -0.000000000000000000, 0.000000000000000000 ) ) ;
#10511 = DIRECTION ( 'NONE',  ( 0.000000000000000000, 0.000000000000000000, 1.000000000000000000 ) ) ;
#10512 = CARTESIAN_POINT ( 'NONE',  ( 0.000000000000000000, -42.79754323328189969, -13.90576474687263264 ) ) ;
#10513 = ORIENTED_EDGE ( 'NONE', *, *, #2252, .T. ) ;
#10514 = EDGE_CURVE ( 'NONE', #906, #8275, #2057, .T. ) ;
#10515 = EDGE_CURVE ( 'NONE', #10912, #15870, #7863, .T. ) ;
#10516 = CIRCLE ( 'NONE', #15391, 24.00000000002400569 ) ;
#10517 = VECTOR ( 'NONE', #8299, 1000.000000000000000 ) ;
#10518 = AXIS2_PLACEMENT_3D ( 'NONE', #11159, #14028, #17271 ) ;
#10519 = DIRECTION ( 'NONE',  ( 0.000000000000000000, -0.9510565162951500895, -0.3090169943749581649 ) ) ;
#10520 = EDGE_CURVE ( 'NONE', #5770, #8874, #1861, .T. ) ;
#10521 = CYLINDRICAL_SURFACE ( 'NONE', #4715, 63.00000000006298961 ) ;
#10522 = CIRCLE ( 'NONE', #2913, 150.0000000000000284 ) ;
#10524 = AXIS2_PLACEMENT_3D ( 'NONE', #16968, #7050, #3924 ) ;
#10523 = DIRECTION ( 'NONE',  ( -1.000000000000000000, 0.000000000000000000, 0.000000000000000000 ) ) ;
#10525 = EDGE_CURVE ( 'NONE', #743, #11942, #11610, .T. ) ;
#10526 = ORIENTED_EDGE ( 'NONE', *, *, #18085, .F. ) ;
#10527 = CARTESIAN_POINT ( 'NONE',  ( 0.000000000000000000, 56.37237871411035428, -1.017308535511785683 ) ) ;
#10528 = ORIENTED_EDGE ( 'NONE', *, *, #14289, .F. ) ;
#10529 = UNCERTAINTY_MEASURE_WITH_UNIT (LENGTH_MEASURE( 1.000000000000000082E-05 ), #2225, 'distance_accuracy_value', 'NONE');
#10530 = CARTESIAN_POINT ( 'NONE',  ( 10.00000000000000000, 31.97297851452424311, 46.27827401617415148 ) ) ;
#10531 = ORIENTED_EDGE ( 'NONE', *, *, #12620, .T. ) ;
#10532 = DIRECTION ( 'NONE',  ( -1.000000000000000000, -0.000000000000000000, -0.000000000000000000 ) ) ;
#10533 = DIRECTION ( 'NONE',  ( 0.000000000000000000, 0.000000000000000000, -1.000000000000000000 ) ) ;
#10534 = AXIS2_PLACEMENT_3D ( 'NONE', #17850, #4803, #5941 ) ;
#10535 = ORIENTED_EDGE ( 'NONE', *, *, #889, .F. ) ;
#10536 = VERTEX_POINT ( 'NONE', #11480 ) ;
#10537 = VECTOR ( 'NONE', #17991, 1000.000000000000000 ) ;
#10538 = CYLINDRICAL_SURFACE ( 'NONE', #2600, 2.649999999999992806 ) ;
#10539 = AXIS2_PLACEMENT_3D ( 'NONE', #9617, #12867, #11040 ) ;
#10540 = ORIENTED_EDGE ( 'NONE', *, *, #1904, .F. ) ;
#10541 = DIRECTION ( 'NONE',  ( 0.000000000000000000, 0.000000000000000000, 1.000000000000000000 ) ) ;
#10542 = AXIS2_PLACEMENT_3D ( 'NONE', #1354, #14107, #12976 ) ;
#10543 = CIRCLE ( 'NONE', #6901, 2.649999999999995914 ) ;
#10544 = CARTESIAN_POINT ( 'NONE',  ( -90.00000000009003998, 1.000000000000018208, -5.746271514173173500E-15 ) ) ;
#10545 = AXIS2_PLACEMENT_3D ( 'NONE', #18090, #15433, #2562 ) ;
#10546 = EDGE_CURVE ( 'NONE', #1880, #192, #15564, .T. ) ;
#10547 = ORIENTED_EDGE ( 'NONE', *, *, #13030, .T. ) ;
#10548 = VECTOR ( 'NONE', #13987, 1000.000000000000000 ) ;
#10549 = CIRCLE ( 'NONE', #7802, 25.00000000000000000 ) ;
#10550 = VERTEX_POINT ( 'NONE', #2521 ) ;
#10551 = FACE_OUTER_BOUND ( 'NONE', #17550, .T. ) ;
#10552 = CIRCLE ( 'NONE', #8127, 27.00000000000000355 ) ;
#10553 = DIRECTION ( 'NONE',  ( 0.000000000000000000, 0.000000000000000000, -1.000000000000000000 ) ) ;
#10554 = DIRECTION ( 'NONE',  ( 0.000000000000000000, 0.000000000000000000, -1.000000000000000000 ) ) ;
#10555 = ORIENTED_EDGE ( 'NONE', *, *, #5872, .F. ) ;
#10556 = CARTESIAN_POINT ( 'NONE',  ( -26.29305231718584324, -26.50000000000000000, 19.10302069950530779 ) ) ;
#10557 = LINE ( 'NONE', #16377, #15788 ) ;
#10558 = DIRECTION ( 'NONE',  ( 0.000000000000000000, 0.000000000000000000, 1.000000000000000000 ) ) ;
#10559 = DIRECTION ( 'NONE',  ( 1.000000000000000000, 0.000000000000000000, 0.000000000000000000 ) ) ;
#10560 = VERTEX_POINT ( 'NONE', #12908 ) ;
#10561 = CYLINDRICAL_SURFACE ( 'NONE', #16116, 1.250000000000001110 ) ;
#10562 = EDGE_LOOP ( 'NONE', ( #16584, #12082, #9977, #14320 ) ) ;
#10563 = CARTESIAN_POINT ( 'NONE',  ( 10.00000000000000000, 50.69000562871642046, -24.68609584167177218 ) ) ;
#10564 = DIRECTION ( 'NONE',  ( 0.000000000000000000, 0.000000000000000000, 1.000000000000000000 ) ) ;
#10565 = VECTOR ( 'NONE', #453, 1000.000000000000000 ) ;
#10566 = AXIS2_PLACEMENT_3D ( 'NONE', #17945, #4699, #13283 ) ;
#10567 = AXIS2_PLACEMENT_3D ( 'NONE', #15204, #2145, #249 ) ;
#10568 = VECTOR ( 'NONE', #1453, 1000.000000000000000 ) ;
#10569 = EDGE_CURVE ( 'NONE', #10049, #7314, #11375, .T. ) ;
#10570 = ORIENTED_EDGE ( 'NONE', *, *, #1909, .T. ) ;
#10571 = CARTESIAN_POINT ( 'NONE',  ( -90.00000000009003998, 1.821459649775647449E-14, -5.746271514173173500E-15 ) ) ;
#10572 = CIRCLE ( 'NONE', #6002, 26.24900000002624978 ) ;
#10573 = EDGE_LOOP ( 'NONE', ( #16613, #7059 ) ) ;
#10574 = DIRECTION ( 'NONE',  ( 0.000000000000000000, -0.1564344650402382242, 0.9876883405951364381 ) ) ;
#10575 = AXIS2_PLACEMENT_3D ( 'NONE', #2420, #16799, #7934 ) ;
#10576 = DIRECTION ( 'NONE',  ( -1.000000000000000000, -0.000000000000000000, -0.000000000000000000 ) ) ;
#10577 = DIRECTION ( 'NONE',  ( 0.000000000000000000, 0.000000000000000000, 1.000000000000000000 ) ) ;
#10578 = AXIS2_PLACEMENT_3D ( 'NONE', #5571, #11374, #10771 ) ;
#10579 = CARTESIAN_POINT ( 'NONE',  ( 21.00000000000000355, 0.000000000000000000, 0.000000000000000000 ) ) ;
#10580 = ORIENTED_EDGE ( 'NONE', *, *, #18550, .T. ) ;
#10581 = AXIS2_PLACEMENT_3D ( 'NONE', #9811, #15533, #5328 ) ;
#10582 = CYLINDRICAL_SURFACE ( 'NONE', #18527, 24.00000000002399858 ) ;
#10583 = EDGE_LOOP ( 'NONE', ( #5712, #2829, #5494, #9506 ) ) ;
#10584 = PRODUCT_DEFINITION_SHAPE ( 'NONE', 'NONE',  #8047 ) ;
#10585 = CARTESIAN_POINT ( 'NONE',  ( 10.00000000000000000, -46.27827401617427228, 31.97297851452409034 ) ) ;
#10586 = EDGE_LOOP ( 'NONE', ( #4861, #13303, #14639, #4090 ) ) ;
#10587 = EDGE_CURVE ( 'NONE', #18014, #12293, #7939, .T. ) ;
#10588 = ORIENTED_EDGE ( 'NONE', *, *, #10793, .F. ) ;
#10589 = VECTOR ( 'NONE', #13304, 1000.000000000000000 ) ;
#10590 = AXIS2_PLACEMENT_3D ( 'NONE', #8597, #6991, #9935 ) ;
#10591 = EDGE_CURVE ( 'NONE', #2530, #872, #4249, .T. ) ;
#10592 = ORIENTED_EDGE ( 'NONE', *, *, #7965, .T. ) ;
#10593 = AXIS2_PLACEMENT_3D ( 'NONE', #17986, #1979, #13616 ) ;
#10594 = ORIENTED_EDGE ( 'NONE', *, *, #44, .T. ) ;
#10595 = DIRECTION ( 'NONE',  ( -1.000000000000000000, -0.000000000000000000, -0.000000000000000000 ) ) ;
#10596 =( NAMED_UNIT ( * ) PLANE_ANGLE_UNIT ( ) SI_UNIT ( $, .RADIAN. ) );
#10597 = DIRECTION ( 'NONE',  ( 0.000000000000000000, 0.000000000000000000, -1.000000000000000000 ) ) ;
#10598 = FACE_OUTER_BOUND ( 'NONE', #2291, .T. ) ;
#10599 = CARTESIAN_POINT ( 'NONE',  ( 0.000000000000000000, -53.06836994729246726, 18.64666490672351529 ) ) ;
#10600 = CIRCLE ( 'NONE', #1505, 12.00000000001200462 ) ;
#10601 = DIRECTION ( 'NONE',  ( 0.000000000000000000, 0.000000000000000000, 1.000000000000000000 ) ) ;
#10602 = CARTESIAN_POINT ( 'NONE',  ( 11.14999999999999680, 0.000000000000000000, 0.000000000000000000 ) ) ;
#10603 = ORIENTED_EDGE ( 'NONE', *, *, #11222, .T. ) ;
#10604 = CARTESIAN_POINT ( 'NONE',  ( 5.000000000000000000, -57.83923611457337444, 24.97244012287480430 ) ) ;
#10605 = ORIENTED_EDGE ( 'NONE', *, *, #8434, .T. ) ;
#10606 = CIRCLE ( 'NONE', #17600, 0.2500000000000002220 ) ;
#10607 = EDGE_CURVE ( 'NONE', #8897, #2152, #14646, .T. ) ;
#10608 = DIRECTION ( 'NONE',  ( 0.000000000000000000, 0.000000000000000000, -1.000000000000000000 ) ) ;
#10609 = CARTESIAN_POINT ( 'NONE',  ( 4.249769933734876659, -30.10148593525447680, -2.000000000000000000 ) ) ;
#10610 = VECTOR ( 'NONE', #770, 1000.000000000000000 ) ;
#10611 = EDGE_LOOP ( 'NONE', ( #2333, #7906, #2687, #16858 ) ) ;
#10612 = ORIENTED_EDGE ( 'NONE', *, *, #15431, .F. ) ;
#10613 = FACE_OUTER_BOUND ( 'NONE', #10433, .T. ) ;
#10614 = DIRECTION ( 'NONE',  ( -1.000000000000000000, 0.000000000000000000, 0.000000000000000000 ) ) ;
#10615 = DIRECTION ( 'NONE',  ( -1.000000000000000000, 0.000000000000000000, 0.000000000000000000 ) ) ;
#10616 = ORIENTED_EDGE ( 'NONE', *, *, #14651, .F. ) ;
#10617 = AXIS2_PLACEMENT_3D ( 'NONE', #16683, #5240, #2393 ) ;
#10618 = CYLINDRICAL_SURFACE ( 'NONE', #11104, 63.00000000006298961 ) ;
#10619 = FACE_BOUND ( 'NONE', #1654, .T. ) ;
#10620 = CARTESIAN_POINT ( 'NONE',  ( 10.00000000000000000, 48.50907078259382388, 40.19788616105626744 ) ) ;
#10621 = EDGE_LOOP ( 'NONE', ( #6285, #11063, #10217, #4598 ) ) ;
#10622 = DIRECTION ( 'NONE',  ( 1.000000000000000000, 0.000000000000000000, 0.000000000000000000 ) ) ;
#10623 = ORIENTED_EDGE ( 'NONE', *, *, #8212, .T. ) ;
#10624 = CARTESIAN_POINT ( 'NONE',  ( 0.000000000000000000, 9.514709542737238124, -24.46385708179973406 ) ) ;
#10625 = ORIENTED_EDGE ( 'NONE', *, *, #6119, .F. ) ;
#10626 = ADVANCED_FACE ( 'NONE', ( #18529 ), #10136, .T. ) ;
#10627 = ADVANCED_FACE ( 'NONE', ( #14419 ), #2433, .T. ) ;
#10628 = EDGE_CURVE ( 'NONE', #14866, #9218, #2163, .T. ) ;
#10629 = CARTESIAN_POINT ( 'NONE',  ( 2.500000000000000000, 1.768423874527822903, -1.021000000000002350 ) ) ;
#10630 = CARTESIAN_POINT ( 'NONE',  ( 0.000000000000000000, -48.50907078259410099, 40.19788616105593348 ) ) ;
#10631 = AXIS2_PLACEMENT_3D ( 'NONE', #6179, #13430, #288 ) ;
#10632 = VERTEX_POINT ( 'NONE', #9856 ) ;
#10633 = ORIENTED_EDGE ( 'NONE', *, *, #16346, .T. ) ;
#10634 = DIRECTION ( 'NONE',  ( 0.000000000000000000, 0.000000000000000000, 1.000000000000000000 ) ) ;
#10635 = AXIS2_PLACEMENT_3D ( 'NONE', #446, #16741, #13503 ) ;
#10636 = EDGE_CURVE ( 'NONE', #10019, #5831, #5664, .T. ) ;
#10637 = ORIENTED_EDGE ( 'NONE', *, *, #8986, .F. ) ;
#10638 = CARTESIAN_POINT ( 'NONE',  ( 0.000000000000000000, 1.178949249685212974, -2.042000000000001148 ) ) ;
#10639 = EDGE_CURVE ( 'NONE', #1486, #4499, #13403, .T. ) ;
#10640 = ADVANCED_FACE ( 'NONE', ( #5380 ), #11186, .T. ) ;
#10641 = EDGE_CURVE ( 'NONE', #5795, #701, #2178, .T. ) ;
#10642 = DIRECTION ( 'NONE',  ( 0.000000000000000000, 0.000000000000000000, 1.000000000000000000 ) ) ;
#10643 = AXIS2_PLACEMENT_3D ( 'NONE', #1209, #4257, #7008 ) ;
#10644 = ORIENTED_EDGE ( 'NONE', *, *, #12490, .T. ) ;
#10645 = AXIS2_PLACEMENT_3D ( 'NONE', #4410, #3173, #16037 ) ;
#10646 = EDGE_LOOP ( 'NONE', ( #4613, #828, #14584, #83 ) ) ;
#10647 = DIRECTION ( 'NONE',  ( -1.000000000000000000, -0.000000000000000000, 0.000000000000000000 ) ) ;
#10648 = CARTESIAN_POINT ( 'NONE',  ( 0.000000000000000000, 15.00000000000000000, 0.000000000000000000 ) ) ;
#10649 = CARTESIAN_POINT ( 'NONE',  ( 5.000000000000000000, 54.20017844242556748, -32.11449294037138458 ) ) ;
#10650 = ORIENTED_EDGE ( 'NONE', *, *, #7041, .T. ) ;
#10651 = CARTESIAN_POINT ( 'NONE',  ( 10.00000000000000000, 0.000000000000000000, 0.000000000000000000 ) ) ;
#10652 = EDGE_CURVE ( 'NONE', #596, #8275, #3095, .T. ) ;
#10653 = CYLINDRICAL_SURFACE ( 'NONE', #5133, 27.29487558977753991 ) ;
#10654 = DIRECTION ( 'NONE',  ( -1.000000000000000000, 2.312964634635740492E-16, 0.000000000000000000 ) ) ;
#10655 = CARTESIAN_POINT ( 'NONE',  ( 4.203833317240879275, 1.627343821129582979, -3.597273115243889929 ) ) ;
#10656 = VERTEX_POINT ( 'NONE', #17107 ) ;
#10657 = DIRECTION ( 'NONE',  ( -1.000000000000000000, 0.000000000000000000, -0.000000000000000000 ) ) ;
#10658 = B_SPLINE_CURVE_WITH_KNOTS ( 'NONE', 3,
 ( #13259, #14773, #11835, #1728, #12107 ),
 .UNSPECIFIED., .F., .F.,
 ( 4, 1, 4 ),
 ( 0.000000000000000000, 0.002309401076758506657, 0.004618802153517013315 ),
 .UNSPECIFIED. ) ;
#10659 = VERTEX_POINT ( 'NONE', #4056 ) ;
#10660 = FACE_OUTER_BOUND ( 'NONE', #8081, .T. ) ;
#10661 = CARTESIAN_POINT ( 'NONE',  ( -90.40159941089927997, -49.14213562373095812, -4.983845695167307355 ) ) ;
#10662 = EDGE_CURVE ( 'NONE', #13907, #2471, #15665, .T. ) ;
#10663 = AXIS2_PLACEMENT_3D ( 'NONE', #6783, #6872, #8117 ) ;
#10664 = ORIENTED_EDGE ( 'NONE', *, *, #11405, .F. ) ;
#10665 = CARTESIAN_POINT ( 'NONE',  ( 2.500000000000000000, -1.768423874527825568, -1.020999999999998575 ) ) ;
#10666 = VERTEX_POINT ( 'NONE', #17194 ) ;
#10667 = DIRECTION ( 'NONE',  ( 0.000000000000000000, 0.000000000000000000, -1.000000000000000000 ) ) ;
#10668 = DIRECTION ( 'NONE',  ( -1.000000000000000000, 0.000000000000000000, 0.000000000000000000 ) ) ;
#10669 = CIRCLE ( 'NONE', #4900, 26.24900000002626044 ) ;
#10670 = CARTESIAN_POINT ( 'NONE',  ( 5.000000000000000000, -15.68049343256016570, 29.03656532225557996 ) ) ;
#10671 = CARTESIAN_POINT ( 'NONE',  ( -23.48826165280196321, 11.24999999999999467, -0.7426739052322690604 ) ) ;
#10672 = CARTESIAN_POINT ( 'NONE',  ( 10.00000000000000000, 18.38754094778314752, -53.29895248911656580 ) ) ;
#10673 = ORIENTED_EDGE ( 'NONE', *, *, #11592, .F. ) ;
#10674 = DIRECTION ( 'NONE',  ( 1.000000000000000000, 0.000000000000000000, 0.000000000000000000 ) ) ;
#10675 = CARTESIAN_POINT ( 'NONE',  ( -4.197393957002303999, 0.4069871074557429025, -3.503767560748926257 ) ) ;
#10676 = EDGE_LOOP ( 'NONE', ( #11780, #17781, #12552, #6690 ) ) ;
#10677 = EDGE_CURVE ( 'NONE', #15251, #7427, #11868, .T. ) ;
#10678 = EDGE_LOOP ( 'NONE', ( #10727, #13192, #1401, #4358 ) ) ;
#10679 = ORIENTED_EDGE ( 'NONE', *, *, #13646, .T. ) ;
#10680 = VERTEX_POINT ( 'NONE', #5573 ) ;
#10681 = CARTESIAN_POINT ( 'NONE',  ( 0.000000000000000000, 22.76987570971561681, -23.88582760061456511 ) ) ;
#10682 = DIRECTION ( 'NONE',  ( -1.000000000000000000, -0.000000000000000000, -0.000000000000000000 ) ) ;
#10683 = CARTESIAN_POINT ( 'NONE',  ( -2.688821387764050996E-14, -4.618802153517012954, -0.4999999999999995559 ) ) ;
#10684 = EDGE_CURVE ( 'NONE', #2059, #7314, #9952, .T. ) ;
#10685 = LINE ( 'NONE', #9255, #11439 ) ;
#10686 = LINE ( 'NONE', #5166, #16418 ) ;
#10687 = DIRECTION ( 'NONE',  ( -0.000000000000000000, 0.000000000000000000, 1.000000000000000000 ) ) ;
#10688 = DIRECTION ( 'NONE',  ( 0.000000000000000000, 1.000000000000000000, -1.103561164596346103E-15 ) ) ;
#10689 = DIRECTION ( 'NONE',  ( -1.000000000000000000, -0.000000000000000000, 0.000000000000000000 ) ) ;
#10690 = ORIENTED_EDGE ( 'NONE', *, *, #15810, .F. ) ;
#10691 = PLANE ( 'NONE',  #11527 ) ;
#10692 = ORIENTED_EDGE ( 'NONE', *, *, #15521, .T. ) ;
#10693 = EDGE_CURVE ( 'NONE', #1171, #6377, #10951, .T. ) ;
#10694 = CYLINDRICAL_SURFACE ( 'NONE', #3226, 56.24900000005625600 ) ;
#10695 = DIRECTION ( 'NONE',  ( -1.000000000000000000, -0.000000000000000000, 0.000000000000000000 ) ) ;
#10696 = CARTESIAN_POINT ( 'NONE',  ( -79.64793068852927149, -34.99999999999999289, 31.86039329588764701 ) ) ;
#10697 = ORIENTED_EDGE ( 'NONE', *, *, #13957, .F. ) ;
#10698 = ORIENTED_EDGE ( 'NONE', *, *, #1909, .F. ) ;
#10699 = DIRECTION ( 'NONE',  ( 0.000000000000000000, -0.3090169943749349057, -0.9510565162951576390 ) ) ;
#10700 = DIRECTION ( 'NONE',  ( 6.123233995736766036E-17, -1.000000000000000000, 0.000000000000000000 ) ) ;
#10701 = CIRCLE ( 'NONE', #18002, 1.249999999999999778 ) ;
#10702 = CARTESIAN_POINT ( 'NONE',  ( 10.00000000000000000, 49.76630880786347433, -26.49895292617950560 ) ) ;
#10703 = ORIENTED_EDGE ( 'NONE', *, *, #16831, .F. ) ;
#10704 = CARTESIAN_POINT ( 'NONE',  ( -10.00000000000000000, 26.45033635316149301, 36.40576474687247099 ) ) ;
#10705 = CARTESIAN_POINT ( 'NONE',  ( -5.032868406504333869, -28.36021363089093938, -2.000000000000000000 ) ) ;
#10706 = DIRECTION ( 'NONE',  ( -1.000000000000000000, 0.000000000000000000, 0.000000000000000000 ) ) ;
#10707 = VERTEX_POINT ( 'NONE', #1839 ) ;
#10708 = DIRECTION ( 'NONE',  ( 0.000000000000000000, 0.000000000000000000, -1.000000000000000000 ) ) ;
#10709 = ORIENTED_EDGE ( 'NONE', *, *, #12272, .T. ) ;
#10710 = DIRECTION ( 'NONE',  ( 0.000000000000000000, 0.8090169943749445647, 0.5877852522924770229 ) ) ;
#10711 = VERTEX_POINT ( 'NONE', #1562 ) ;
#10712 =( REPRESENTATION_RELATIONSHIP ('NONE','NONE', #11014, #8256 ) REPRESENTATION_RELATIONSHIP_WITH_TRANSFORMATION ( #1831 )SHAPE_REPRESENTATION_RELATIONSHIP( ) );
#10713 = FACE_OUTER_BOUND ( 'NONE', #12494, .T. ) ;
#10714 = DIRECTION ( 'NONE',  ( 0.000000000000000000, 0.000000000000000000, 1.000000000000000000 ) ) ;
#10715 = ORIENTED_EDGE ( 'NONE', *, *, #16992, .F. ) ;
#10716 = EDGE_LOOP ( 'NONE', ( #13462, #13690 ) ) ;
#10717 = DIRECTION ( 'NONE',  ( 0.000000000000000000, 0.000000000000000000, 1.000000000000000000 ) ) ;
#10718 =( NAMED_UNIT ( * ) PLANE_ANGLE_UNIT ( ) SI_UNIT ( $, .RADIAN. ) );
#10719 = VERTEX_POINT ( 'NONE', #11845 ) ;
#10720 = LINE ( 'NONE', #2343, #4250 ) ;
#10721 = VECTOR ( 'NONE', #3772, 1000.000000000000000 ) ;
#10722 = VECTOR ( 'NONE', #14031, 1000.000000000000000 ) ;
#10723 = CIRCLE ( 'NONE', #12883, 0.7499999999999997780 ) ;
#10724 = ADVANCED_FACE ( 'NONE', ( #17466 ), #325, .T. ) ;
#10725 = DIRECTION ( 'NONE',  ( 0.000000000000000000, 0.000000000000000000, 1.000000000000000000 ) ) ;
#10726 = ADVANCED_FACE ( 'NONE', ( #6029 ), #7555, .T. ) ;
#10727 = ORIENTED_EDGE ( 'NONE', *, *, #6803, .F. ) ;
#10728 = EDGE_CURVE ( 'NONE', #16959, #5879, #4609, .T. ) ;
#10729 = PRODUCT_DEFINITION_SHAPE ( 'NONE', 'NONE',  #18843 ) ;
#10730 = ORIENTED_EDGE ( 'NONE', *, *, #5274, .T. ) ;
#10731 = DIRECTION ( 'NONE',  ( 0.000000000000000000, 0.000000000000000000, 1.000000000000000000 ) ) ;
#10732 = CARTESIAN_POINT ( 'NONE',  ( -117.1020693116506379, -34.99999999999999289, -19.69080595179801207 ) ) ;
#10733 = CARTESIAN_POINT ( 'NONE',  ( 10.00000000000000000, -53.06836994729246726, 18.64666490672351529 ) ) ;
#10734 = ORIENTED_EDGE ( 'NONE', *, *, #3433, .T. ) ;
#10735 = CARTESIAN_POINT ( 'NONE',  ( 5.000000000000000000, 23.24033432160437584, 58.55669782892469755 ) ) ;
#10736 = EDGE_CURVE ( 'NONE', #3305, #18793, #4789, .T. ) ;
#10737 = CIRCLE ( 'NONE', #5275, 25.00000000000000000 ) ;
#10738 = DIRECTION ( 'NONE',  ( 0.000000000000000000, 0.5877852522924742473, -0.8090169943749465631 ) ) ;
#10739 = FACE_OUTER_BOUND ( 'NONE', #17737, .T. ) ;
#10740 = DIRECTION ( 'NONE',  ( -1.000000000000000000, 0.000000000000000000, -0.000000000000000000 ) ) ;
#10741 = EDGE_LOOP ( 'NONE', ( #822, #1214, #16732, #15576 ) ) ;
#10742 = SURFACE_SIDE_STYLE ('',( #1891 ) ) ;
#10744 = EDGE_CURVE ( 'NONE', #15168, #8023, #13735, .T. ) ;
#10743 = ORIENTED_EDGE ( 'NONE', *, *, #6450, .T. ) ;
#10745 = DIRECTION ( 'NONE',  ( -0.000000000000000000, -0.000000000000000000, 1.000000000000000000 ) ) ;
#10746 = LINE ( 'NONE', #667, #18347 ) ;
#10747 = EDGE_CURVE ( 'NONE', #16839, #5310, #5535, .T. ) ;
#10748 = AXIS2_PLACEMENT_3D ( 'NONE', #707, #11064, #6608 ) ;
#10749 = EDGE_CURVE ( 'NONE', #10364, #4317, #12171, .T. ) ;
#10750 = ORIENTED_EDGE ( 'NONE', *, *, #14958, .F. ) ;
#10751 = EDGE_CURVE ( 'NONE', #8784, #18371, #7047, .T. ) ;
#10752 = ORIENTED_EDGE ( 'NONE', *, *, #9820, .T. ) ;
#10753 = PLANE ( 'NONE',  #17602 ) ;
#10755 = EDGE_CURVE ( 'NONE', #15153, #4463, #17691, .T. ) ;
#10754 = CARTESIAN_POINT ( 'NONE',  ( -31.74999999999995737, 5.204748896376250699E-16, -4.250000000000000000 ) ) ;
#10756 = LINE ( 'NONE', #10848, #8427 ) ;
#10757 = DIRECTION ( 'NONE',  ( -1.000000000000000000, -0.000000000000000000, -0.000000000000000000 ) ) ;
#10758 = CARTESIAN_POINT ( 'NONE',  ( -0.3865131578947368918, -23.49682122285426189, 0.000000000000000000 ) ) ;
#10759 = VERTEX_POINT ( 'NONE', #2895 ) ;
#10760 = CARTESIAN_POINT ( 'NONE',  ( 0.000000000000000000, 27.72801475327282361, -5.086963483077305170 ) ) ;
#10761 =( NAMED_UNIT ( * ) SI_UNIT ( $, .STERADIAN. ) SOLID_ANGLE_UNIT ( ) );
#10762 = CARTESIAN_POINT ( 'NONE',  ( -290.0000000000001137, -30.00000000000000000, -125.0000000000000000 ) ) ;
#10763 = ORIENTED_EDGE ( 'NONE', *, *, #11101, .F. ) ;
#10764 = ITEM_DEFINED_TRANSFORMATION ( 'NONE', 'NONE', #12926,  #8017 ) ;
#10765 = VERTEX_POINT ( 'NONE', #10326 ) ;
#10766 = ORIENTED_EDGE ( 'NONE', *, *, #4251, .F. ) ;
#10767 = ORIENTED_EDGE ( 'NONE', *, *, #15757, .F. ) ;
#10768 = DIRECTION ( 'NONE',  ( -1.000000000000000000, -0.000000000000000000, 0.000000000000000000 ) ) ;
#10769 = DIRECTION ( 'NONE',  ( 0.000000000000000000, -1.224646799147334718E-16, 1.000000000000000000 ) ) ;
#10770 = ADVANCED_BREP_SHAPE_REPRESENTATION ( '', ( #3564, #8017 ), #3170 ) ;
#10771 = DIRECTION ( 'NONE',  ( 0.000000000000000000, -0.3090169943749350723, -0.9510565162951576390 ) ) ;
#10772 = ADVANCED_FACE ( 'NONE', ( #1476 ), #7451, .F. ) ;
#10773 = CARTESIAN_POINT ( 'NONE',  ( -4.144923636027600722, -29.35885059145708098, -2.000000000000000000 ) ) ;
#10774 = DIRECTION ( 'NONE',  ( -1.000000000000000000, -0.000000000000000000, -0.000000000000000000 ) ) ;
#10775 = LINE ( 'NONE', #17660, #17430 ) ;
#10776 = FACE_OUTER_BOUND ( 'NONE', #13942, .T. ) ;
#10777 = ORIENTED_EDGE ( 'NONE', *, *, #6097, .F. ) ;
#10778 = CARTESIAN_POINT ( 'NONE',  ( 10.00000000000000000, -22.07705612348828694, -14.19907017806892569 ) ) ;
#10779 = VERTEX_POINT ( 'NONE', #14513 ) ;
#10780 = DIRECTION ( 'NONE',  ( 1.000000000000000000, -0.000000000000000000, -0.000000000000000000 ) ) ;
#10781 = LINE ( 'NONE', #6131, #12582 ) ;
#10782 = DIRECTION ( 'NONE',  ( 1.000000000000000000, 0.000000000000000000, -0.000000000000000000 ) ) ;
#10783 = ORIENTED_EDGE ( 'NONE', *, *, #7148, .T. ) ;
#10784 = EDGE_LOOP ( 'NONE', ( #11693, #8829, #10942, #3165 ) ) ;
#10785 = DIRECTION ( 'NONE',  ( -1.000000000000000000, -0.000000000000000000, -0.000000000000000000 ) ) ;
#10786 = DIRECTION ( 'NONE',  ( 0.000000000000000000, 0.000000000000000000, 1.000000000000000000 ) ) ;
#10787 = AXIS2_PLACEMENT_3D ( 'NONE', #2602, #1191, #9552 ) ;
#10788 = CARTESIAN_POINT ( 'NONE',  ( 0.000000000000000000, 0.000000000000000000, 0.000000000000000000 ) ) ;
#10789 = ORIENTED_EDGE ( 'NONE', *, *, #13180, .T. ) ;
#10790 = VECTOR ( 'NONE', #2537, 1000.000000000000000 ) ;
#10791 = CIRCLE ( 'NONE', #1074, 33.00000000003299760 ) ;
#10792 = EDGE_CURVE ( 'NONE', #17281, #3888, #1533, .T. ) ;
#10793 = EDGE_CURVE ( 'NONE', #15209, #435, #8883, .T. ) ;
#10794 = CARTESIAN_POINT ( 'NONE',  ( 0.000000000000000000, -3.730438010304518492, 27.94286728106391138 ) ) ;
#10795 = CYLINDRICAL_SURFACE ( 'NONE', #5165, 24.00000000002399503 ) ;
#10796 = VECTOR ( 'NONE', #16257, 1000.000000000000000 ) ;
#10797 = CARTESIAN_POINT ( 'NONE',  ( 10.04305231718579705, -26.50000000000000000, 30.90933677959249337 ) ) ;
#10798 = ORIENTED_EDGE ( 'NONE', *, *, #15478, .T. ) ;
#10799 = LINE ( 'NONE', #16623, #18286 ) ;
#10800 = PRODUCT_DEFINITION_FORMATION_WITH_SPECIFIED_SOURCE ( 'ANY', '', #8742, .NOT_KNOWN. ) ;
#10801 = ORIENTED_EDGE ( 'NONE', *, *, #13733, .T. ) ;
#10802 = CARTESIAN_POINT ( 'NONE',  ( 50.00005079999999680, 0.000000000000000000, 0.000000000000000000 ) ) ;
#10803 = AXIS2_PLACEMENT_3D ( 'NONE', #17543, #14593, #1630 ) ;
#10804 = ORIENTED_EDGE ( 'NONE', *, *, #4089, .F. ) ;
#10805 = CARTESIAN_POINT ( 'NONE',  ( 1.312671235360372224, 3.860931062424219462, -0.05923475698270440348 ) ) ;
#10806 = DIRECTION ( 'NONE',  ( 0.000000000000000000, 0.000000000000000000, 1.000000000000000000 ) ) ;
#10807 = ORIENTED_EDGE ( 'NONE', *, *, #3670, .T. ) ;
#10808 = VERTEX_POINT ( 'NONE', #8967 ) ;
#10809 = DIRECTION ( 'NONE',  ( 1.000000000000000000, 0.000000000000000000, 0.000000000000000000 ) ) ;
#10810 = SHAPE_REPRESENTATION_RELATIONSHIP ( 'NONE' , 'NONE' ,  #13460, #6260 ) ;
#10811 = ORIENTED_EDGE ( 'NONE', *, *, #295, .T. ) ;
#10812 = DIRECTION ( 'NONE',  ( 0.000000000000000000, 0.000000000000000000, 1.000000000000000000 ) ) ;
#10813 = AXIS2_PLACEMENT_3D ( 'NONE', #17392, #1387, #7096 ) ;
#10814 = EDGE_CURVE ( 'NONE', #7932, #5476, #14605, .T. ) ;
#10815 = AXIS2_PLACEMENT_3D ( 'NONE', #969, #18483, #5331 ) ;
#10816 = DIRECTION ( 'NONE',  ( 0.000000000000000000, -0.9876883405951358830, -0.1564344650402420822 ) ) ;
#10817 = DIRECTION ( 'NONE',  ( 0.000000000000000000, 0.000000000000000000, 1.000000000000000000 ) ) ;
#10818 = VERTEX_POINT ( 'NONE', #4691 ) ;
#10819 = ORIENTED_EDGE ( 'NONE', *, *, #283, .F. ) ;
#10820 = CARTESIAN_POINT ( 'NONE',  ( 1.390230914382191596, 4.043987460488659202, -3.502507215260488582 ) ) ;
#10821 = FACE_OUTER_BOUND ( 'NONE', #15946, .T. ) ;
#10823 = AXIS2_PLACEMENT_3D ( 'NONE', #11812, #13150, #11432 ) ;
#10822 = DIRECTION ( 'NONE',  ( 0.000000000000000000, 0.000000000000000000, 1.000000000000000000 ) ) ;
#10824 = VERTEX_POINT ( 'NONE', #14896 ) ;
#10825 = DIRECTION ( 'NONE',  ( -1.000000000000000000, -0.000000000000000000, -0.000000000000000000 ) ) ;
#10826 = DIRECTION ( 'NONE',  ( -0.000000000000000000, -0.000000000000000000, -1.000000000000000000 ) ) ;
#10827 = CARTESIAN_POINT ( 'NONE',  ( 2.500000000000000000, -2.357898499370431722, 2.818925648462311528E-15 ) ) ;
#10828 = AXIS2_PLACEMENT_3D ( 'NONE', #5823, #11549, #8674 ) ;
#10829 = CARTESIAN_POINT ( 'NONE',  ( -2.000000000000007550, -3.464101615137749945, 0.000000000000000000 ) ) ;
#10830 = VERTEX_POINT ( 'NONE', #14610 ) ;
#10831 = CIRCLE ( 'NONE', #2934, 28.00000000000000355 ) ;
#10832 = EDGE_CURVE ( 'NONE', #17331, #16237, #3059, .T. ) ;
#10833 = DIRECTION ( 'NONE',  ( -0.1586811557617541224, 0.000000000000000000, -0.9873298794253690946 ) ) ;
#10834 = EDGE_CURVE ( 'NONE', #2490, #2365, #6393, .T. ) ;
#10835 = ORIENTED_EDGE ( 'NONE', *, *, #15403, .F. ) ;
#10836 = DIRECTION ( 'NONE',  ( -1.000000000000000000, 0.000000000000000000, 0.000000000000000000 ) ) ;
#10837 = DIRECTION ( 'NONE',  ( 0.000000000000000000, 0.000000000000000000, 1.000000000000000000 ) ) ;
#10838=STYLED_ITEM('',(#18883),#3805);
#10839 = CIRCLE ( 'NONE', #3856, 27.00000000000000355 ) ;
#10840 = VECTOR ( 'NONE', #5115, 1000.000000000000000 ) ;
#10841 = AXIS2_PLACEMENT_3D ( 'NONE', #1156, #4009, #17426 ) ;
#10842 = ORIENTED_EDGE ( 'NONE', *, *, #10423, .T. ) ;
#10843 = EDGE_CURVE ( 'NONE', #10448, #941, #621, .T. ) ;
#10844 = ORIENTED_EDGE ( 'NONE', *, *, #5464, .F. ) ;
#10845 = CARTESIAN_POINT ( 'NONE',  ( 10.00000000000000000, 0.000000000000000000, 0.000000000000000000 ) ) ;
#10846 = FACE_OUTER_BOUND ( 'NONE', #8376, .T. ) ;
#10847 = CARTESIAN_POINT ( 'NONE',  ( 2.500000000000000000, 2.357898499370432166, -2.385244779468109755E-15 ) ) ;
#10848 = CARTESIAN_POINT ( 'NONE',  ( -27.29487558977753991, 1.305124410222464393, -2.000000000000000000 ) ) ;
#10849 = DIRECTION ( 'NONE',  ( -0.9914448613738102711, -0.1305261922200524338, 0.000000000000000000 ) ) ;
#10850 = CARTESIAN_POINT ( 'NONE',  ( 0.000000000000000000, -13.79392154159179640, 61.47135697633775209 ) ) ;
#10851 = ORIENTED_EDGE ( 'NONE', *, *, #1244, .F. ) ;
#10852 = CARTESIAN_POINT ( 'NONE',  ( -4.175002511812151873, -2.208363329454905877, -3.469254087858246738 ) ) ;
#10853 = EDGE_CURVE ( 'NONE', #3186, #11686, #7913, .T. ) ;
#10854 = CIRCLE ( 'NONE', #14508, 24.00000000002399503 ) ;
#10855 = ADVANCED_FACE ( 'NONE', ( #901 ), #13742, .T. ) ;
#10856 = EDGE_CURVE ( 'NONE', #6420, #10958, #696, .T. ) ;
#10857 = LINE ( 'NONE', #15166, #6642 ) ;
#10858 = ORIENTED_EDGE ( 'NONE', *, *, #7485, .F. ) ;
#10859 = CIRCLE ( 'NONE', #2662, 63.00000000006298961 ) ;
#10860 = AXIS2_PLACEMENT_3D ( 'NONE', #1564, #7363, #5930 ) ;
#10861 = ITEM_DEFINED_TRANSFORMATION ( 'NONE', 'NONE', #15054,  #8017 ) ;
#10862 = ADVANCED_FACE ( 'NONE', ( #2211 ), #15261, .F. ) ;
#10863 = ORIENTED_EDGE ( 'NONE', *, *, #11386, .F. ) ;
#10864 = ADVANCED_FACE ( 'NONE', ( #10598 ), #2122, .T. ) ;
#10865 = ORIENTED_EDGE ( 'NONE', *, *, #5174, .F. ) ;
#10866 = AXIS2_PLACEMENT_3D ( 'NONE', #2642, #13121, #12928 ) ;
#10867 = ORIENTED_EDGE ( 'NONE', *, *, #13532, .T. ) ;
#10868 = CIRCLE ( 'NONE', #10268, 27.50000000000000000 ) ;
#10869 = EDGE_CURVE ( 'NONE', #3193, #9460, #9933, .T. ) ;
#10870 = DIRECTION ( 'NONE',  ( -1.000000000000000000, 0.000000000000000000, 0.000000000000000000 ) ) ;
#10871 = LINE ( 'NONE', #7829, #3983 ) ;
#10872 = AXIS2_PLACEMENT_3D ( 'NONE', #3833, #12592, #15743 ) ;
#10873 = CARTESIAN_POINT ( 'NONE',  ( -10.00000000000000000, -5.120903701083534543E-13, -42.35000000000000142 ) ) ;
#10874 = DIRECTION ( 'NONE',  ( 0.000000000000000000, 0.000000000000000000, 1.000000000000000000 ) ) ;
#10875 = DIRECTION ( 'NONE',  ( 0.000000000000000000, 1.000000000000000000, 0.000000000000000000 ) ) ;
#10876 = FACE_OUTER_BOUND ( 'NONE', #4215, .T. ) ;
#10877 = DIRECTION ( 'NONE',  ( -1.000000000000000000, -0.000000000000000000, -0.000000000000000000 ) ) ;
#10878 = DIRECTION ( 'NONE',  ( 0.000000000000000000, -0.4999999999999993339, 0.8660254037844390407 ) ) ;
#10879 = ORIENTED_EDGE ( 'NONE', *, *, #3310, .F. ) ;
#10880 = PLANE ( 'NONE',  #13643 ) ;
#10881 = ORIENTED_EDGE ( 'NONE', *, *, #15065, .F. ) ;
#10882 = ADVANCED_FACE ( 'NONE', ( #13826 ), #12300, .T. ) ;
#10883 = CYLINDRICAL_SURFACE ( 'NONE', #10748, 24.00000000002399503 ) ;
#10884 = CARTESIAN_POINT ( 'NONE',  ( 10.00000000000000000, -39.14194549634393638, 40.58063702438330722 ) ) ;
#10885 = AXIS2_PLACEMENT_3D ( 'NONE', #14140, #9561, #17020 ) ;
#10886 = ORIENTED_EDGE ( 'NONE', *, *, #14797, .T. ) ;
#10887 = VERTEX_POINT ( 'NONE', #13935 ) ;
#10888 = DIRECTION ( 'NONE',  ( 0.000000000000000000, 0.1564344650402312575, -0.9876883405951376593 ) ) ;
#10889 = DIRECTION ( 'NONE',  ( 0.000000000000000000, 1.000000000000000000, 0.000000000000000000 ) ) ;
#10890 = VECTOR ( 'NONE', #2885, 1000.000000000000000 ) ;
#10891 = CARTESIAN_POINT ( 'NONE',  ( -1.393927851585477606, 4.043713361053528743, -3.526374918436835149 ) ) ;
#10892 = EDGE_LOOP ( 'NONE', ( #273, #16760, #2158, #15419 ) ) ;
#10893 = MECHANICAL_DESIGN_GEOMETRIC_PRESENTATION_REPRESENTATION (  '', ( #5445 ), #11817 ) ;
#10894 = AXIS2_PLACEMENT_3D ( 'NONE', #18195, #1055, #5536 ) ;
#10895 = EDGE_CURVE ( 'NONE', #3100, #18521, #15102, .T. ) ;
#10896 = FACE_OUTER_BOUND ( 'NONE', #7318, .T. ) ;
#10897 = CARTESIAN_POINT ( 'NONE',  ( 10.00000000000000000, 42.79754323328179311, -16.55576474687299537 ) ) ;
#10898 = CIRCLE ( 'NONE', #2702, 30.39999999999999858 ) ;
#10899 = CARTESIAN_POINT ( 'NONE',  ( -2.100000000000000089, 2.571758278209441957E-16, -0.2800830152838844622 ) ) ;
#10900 = EDGE_LOOP ( 'NONE', ( #4279, #16157, #17146, #2066 ) ) ;
#10901 = CARTESIAN_POINT ( 'NONE',  ( 10.00000000000000000, 0.000000000000000000, 0.000000000000000000 ) ) ;
#10902 = AXIS2_PLACEMENT_3D ( 'NONE', #14954, #1894, #14753 ) ;
#10903 = AXIS2_PLACEMENT_3D ( 'NONE', #10788, #18130, #6424 ) ;
#10904 = CIRCLE ( 'NONE', #7566, 25.00000000000000000 ) ;
#10905 = VERTEX_POINT ( 'NONE', #18113 ) ;
#10906 = AXIS2_PLACEMENT_3D ( 'NONE', #7231, #13054, #10182 ) ;
#10907 = DIRECTION ( 'NONE',  ( 0.000000000000000000, 0.000000000000000000, 1.000000000000000000 ) ) ;
#10908 = ORIENTED_EDGE ( 'NONE', *, *, #1687, .F. ) ;
#10909 = CARTESIAN_POINT ( 'NONE',  ( 11.14999999999999680, 0.000000000000000000, 0.000000000000000000 ) ) ;
#10910 = CARTESIAN_POINT ( 'NONE',  ( -3.500000000000000888, -27.60846790388774608, 0.000000000000000000 ) ) ;
#10911 = ORIENTED_EDGE ( 'NONE', *, *, #10936, .T. ) ;
#10912 = VERTEX_POINT ( 'NONE', #4967 ) ;
#10913 = DIRECTION ( 'NONE',  ( -1.000000000000000000, -0.000000000000000000, -0.000000000000000000 ) ) ;
#10914 = ORIENTED_EDGE ( 'NONE', *, *, #7945, .F. ) ;
#10915 = FACE_OUTER_BOUND ( 'NONE', #1256, .T. ) ;
#10916 = AXIS2_PLACEMENT_3D ( 'NONE', #311, #18199, #9622 ) ;
#10917 = ADVANCED_FACE ( 'NONE', ( #5065 ), #6597, .F. ) ;
#10918 = AXIS2_PLACEMENT_3D ( 'NONE', #666, #570, #12187 ) ;
#10919 = DIRECTION ( 'NONE',  ( -1.000000000000000000, 0.000000000000000000, 0.000000000000000000 ) ) ;
#10920 = LINE ( 'NONE', #4072, #2344 ) ;
#10921 = VERTEX_POINT ( 'NONE', #13653 ) ;
#10922 = CIRCLE ( 'NONE', #16106, 12.00000000001200640 ) ;
#10923 = ORIENTED_EDGE ( 'NONE', *, *, #3716, .F. ) ;
#10924 = FACE_OUTER_BOUND ( 'NONE', #614, .T. ) ;
#10925 = CARTESIAN_POINT ( 'NONE',  ( -26.29305231718584324, -30.00000000000000000, 19.10302069950530779 ) ) ;
#10926 = DIRECTION ( 'NONE',  ( -1.000000000000000000, -0.000000000000000000, -0.000000000000000000 ) ) ;
#10927 = EDGE_CURVE ( 'NONE', #5529, #4919, #8412, .T. ) ;
#10928 = ORIENTED_EDGE ( 'NONE', *, *, #1856, .T. ) ;
#10929 = CARTESIAN_POINT ( 'NONE',  ( -12.50000000000000355, 28.00000000000000355, 0.000000000000000000 ) ) ;
#10930 = AXIS2_PLACEMENT_3D ( 'NONE', #5255, #12301, #3462 ) ;
#10931 = LINE ( 'NONE', #6656, #3926 ) ;
#10932 = FACE_OUTER_BOUND ( 'NONE', #9824, .T. ) ;
#10933 = VERTEX_POINT ( 'NONE', #3740 ) ;
#10934 = VERTEX_POINT ( 'NONE', #15348 ) ;
#10935 = FACE_OUTER_BOUND ( 'NONE', #9562, .T. ) ;
#10936 = EDGE_CURVE ( 'NONE', #9002, #1826, #12499, .T. ) ;
#10937 = ORIENTED_EDGE ( 'NONE', *, *, #3881, .T. ) ;
#10938 = CARTESIAN_POINT ( 'NONE',  ( -79.64793068852898728, -34.99999999999999289, -31.86039329588756530 ) ) ;
#10939 = DIRECTION ( 'NONE',  ( 0.9873298794253685395, -1.799126239882930573E-16, -0.1586811557617575918 ) ) ;
#10940 = CIRCLE ( 'NONE', #3651, 24.00000000002399503 ) ;
#10941 = CIRCLE ( 'NONE', #2748, 24.00000000002399148 ) ;
#10942 = ORIENTED_EDGE ( 'NONE', *, *, #8647, .T. ) ;
#10943 = ORIENTED_EDGE ( 'NONE', *, *, #1334, .T. ) ;
#10944 = CARTESIAN_POINT ( 'NONE',  ( 0.000000000000000000, -31.97297851452457351, 46.27827401617392411 ) ) ;
#10945 = CARTESIAN_POINT ( 'NONE',  ( 2.449293598294706513E-15, -30.00000000000000000, -20.00000000000000000 ) ) ;
#10946 = DIRECTION ( 'NONE',  ( 0.000000000000000000, 0.8660254037844380415, -0.5000000000000011102 ) ) ;
#10947 = DIRECTION ( 'NONE',  ( 0.000000000000000000, 1.000000000000000000, 0.000000000000000000 ) ) ;
#10948 = DIRECTION ( 'NONE',  ( 0.000000000000000000, 0.000000000000000000, 1.000000000000000000 ) ) ;
#10949 = FACE_OUTER_BOUND ( 'NONE', #7163, .T. ) ;
#10950 = EDGE_LOOP ( 'NONE', ( #13946, #18430 ) ) ;
#10952 = FACE_OUTER_BOUND ( 'NONE', #14471, .T. ) ;
#10951 = CIRCLE ( 'NONE', #12829, 24.00000000002399858 ) ;
#10953 = VECTOR ( 'NONE', #16111, 1000.000000000000000 ) ;
#10954 = DIRECTION ( 'NONE',  ( -0.000000000000000000, 1.000000000000000000, -0.000000000000000000 ) ) ;
#10955 = ORIENTED_EDGE ( 'NONE', *, *, #12584, .F. ) ;
#10956 = ITEM_DEFINED_TRANSFORMATION ( 'NONE', 'NONE', #10787,  #8017 ) ;
#10957 = VERTEX_POINT ( 'NONE', #9165 ) ;
#10958 = VERTEX_POINT ( 'NONE', #14985 ) ;
#10959 = EDGE_CURVE ( 'NONE', #14866, #16034, #1929, .T. ) ;
#10960 = EDGE_CURVE ( 'NONE', #14062, #7869, #13578, .T. ) ;
#10961 = ORIENTED_EDGE ( 'NONE', *, *, #12813, .T. ) ;
#10962 = VECTOR ( 'NONE', #11010, 1000.000000000000000 ) ;
#10963 = LINE ( 'NONE', #16878, #15418 ) ;
#10964 = EDGE_CURVE ( 'NONE', #6354, #12492, #10685, .T. ) ;
#10965 = FACE_OUTER_BOUND ( 'NONE', #16350, .T. ) ;
#10966 = DIRECTION ( 'NONE',  ( 1.000000000000000000, -2.312964634635740492E-16, 0.000000000000000000 ) ) ;
#10967 = CARTESIAN_POINT ( 'NONE',  ( 10.00000000000000000, 3.730438010304324425, 27.94286728106393980 ) ) ;
#10968 = EDGE_CURVE ( 'NONE', #12492, #3988, #17531, .T. ) ;
#10969 = DIRECTION ( 'NONE',  ( 1.000000000000000000, -2.312964634635740492E-16, 0.000000000000000000 ) ) ;
#10970 = LINE ( 'NONE', #9542, #3735 ) ;
#10971 = CARTESIAN_POINT ( 'NONE',  ( 10.00000000000000000, -53.06836994729219725, -18.64666490672428623 ) ) ;
#10972 = ORIENTED_EDGE ( 'NONE', *, *, #2863, .F. ) ;
#10973 = LINE ( 'NONE', #14225, #2090 ) ;
#10974 = ORIENTED_EDGE ( 'NONE', *, *, #11423, .F. ) ;
#10975 = EDGE_CURVE ( 'NONE', #18363, #15353, #11460, .T. ) ;
#10976 = CARTESIAN_POINT ( 'NONE',  ( 10.00000000000000000, -26.49895292618039377, 49.76630880786299826 ) ) ;
#10977 = CARTESIAN_POINT ( 'NONE',  ( -9.345251662538453630, -28.92794965710190525, 0.000000000000000000 ) ) ;
#10978 = ORIENTED_EDGE ( 'NONE', *, *, #2549, .F. ) ;
#10979 = EDGE_LOOP ( 'NONE', ( #18356, #2442, #457, #17026, #5116, #7246, #17167, #12224, #2899, #13354, #11599, #8803, #12927, #6692, #16051, #14948 ) ) ;
#10980 = CARTESIAN_POINT ( 'NONE',  ( 10.00000000000000000, 0.000000000000000000, 0.000000000000000000 ) ) ;
#10981 = DIRECTION ( 'NONE',  ( 0.000000000000000000, 0.000000000000000000, 1.000000000000000000 ) ) ;
#10982 = DIRECTION ( 'NONE',  ( 1.000000000000000000, 0.000000000000000000, 0.000000000000000000 ) ) ;
#10983 = EDGE_LOOP ( 'NONE', ( #9510, #4996, #13453, #7853 ) ) ;
#10984 = EDGE_CURVE ( 'NONE', #12076, #3708, #1409, .T. ) ;
#10985 = EDGE_CURVE ( 'NONE', #7427, #10989, #1358, .T. ) ;
#10986 = DIRECTION ( 'NONE',  ( 0.000000000000000000, 0.000000000000000000, 1.000000000000000000 ) ) ;
#10987 = DIRECTION ( 'NONE',  ( -0.000000000000000000, 1.000000000000000000, -0.000000000000000000 ) ) ;
#10988 = CARTESIAN_POINT ( 'NONE',  ( -10.00000000000000000, 0.000000000000000000, 0.000000000000000000 ) ) ;
#10989 = VERTEX_POINT ( 'NONE', #5554 ) ;
#10990 = FACE_OUTER_BOUND ( 'NONE', #17138, .T. ) ;
#10991 = ORIENTED_EDGE ( 'NONE', *, *, #13700, .T. ) ;
#10992 = DIRECTION ( 'NONE',  ( 0.000000000000000000, -1.000000000000000000, 0.000000000000000000 ) ) ;
#10993 = ORIENTED_EDGE ( 'NONE', *, *, #10975, .F. ) ;
#10994 = ADVANCED_FACE ( 'NONE', ( #9922 ), #2499, .F. ) ;
#10995 = VECTOR ( 'NONE', #12303, 1000.000000000000000 ) ;
#10996 = CARTESIAN_POINT ( 'NONE',  ( 0.000000000000000000, 0.000000000000000000, 0.000000000000000000 ) ) ;
#10997 = CARTESIAN_POINT ( 'NONE',  ( 0.000000000000000000, 49.76630880786347433, -26.49895292617950560 ) ) ;
#10998 = CARTESIAN_POINT ( 'NONE',  ( 10.00000000000000000, 33.71303790549352186, -53.22058882792160261 ) ) ;
#10999 = ORIENTED_EDGE ( 'NONE', *, *, #3061, .F. ) ;
#11000 = ORIENTED_EDGE ( 'NONE', *, *, #14138, .F. ) ;
#11001 = DIRECTION ( 'NONE',  ( 1.000000000000000000, 0.000000000000000000, 0.000000000000000000 ) ) ;
#11002 =( NAMED_UNIT ( * ) SI_UNIT ( $, .STERADIAN. ) SOLID_ANGLE_UNIT ( ) );
#11003 = ORIENTED_EDGE ( 'NONE', *, *, #11721, .F. ) ;
#11004 = CARTESIAN_POINT ( 'NONE',  ( 10.00000000000000000, -56.23315539212689629, -1.335003989222221410 ) ) ;
#11005 = AXIS2_PLACEMENT_3D ( 'NONE', #14711, #7572, #7468 ) ;
#11006 = CIRCLE ( 'NONE', #8876, 2.649999999999985700 ) ;
#11007 = DIRECTION ( 'NONE',  ( 1.000000000000000000, 0.000000000000000000, 0.000000000000000000 ) ) ;
#11008 = DIRECTION ( 'NONE',  ( 1.000000000000000000, 0.000000000000000000, 0.000000000000000000 ) ) ;
#11009 = ORIENTED_EDGE ( 'NONE', *, *, #13363, .T. ) ;
#11010 = DIRECTION ( 'NONE',  ( 0.000000000000000000, 0.000000000000000000, 1.000000000000000000 ) ) ;
#11011 = ORIENTED_EDGE ( 'NONE', *, *, #11405, .T. ) ;
#11012 = CARTESIAN_POINT ( 'NONE',  ( 0.000000000000000000, 0.000000000000000000, 0.000000000000000000 ) ) ;
#11013 = CARTESIAN_POINT ( 'NONE',  ( 0.000000000000000000, -9.823366686501049827, 55.51919907100648999 ) ) ;
#11014 = SHAPE_REPRESENTATION ( 'MAS-191', ( #5633, #6525, #8949, #3191, #13821, #5624, #16877, #10471, #2273, #12926, #4705, #1968, #448, #15343, #7137, #11993, #11086, #5316, #7744, #18387, #10189, #9565, #15054, #6842, #17485, #6239, #2603, #3515, #4419, #17502, #15068, #14155, #466, #8960, #10787, #7755, #7445, #11412, #18095, #12633 ), #2581 ) ;
#11015 = DIRECTION ( 'NONE',  ( -1.000000000000000000, -0.000000000000000000, 0.000000000000000000 ) ) ;
#11016 = VERTEX_POINT ( 'NONE', #4036 ) ;
#11017 = CARTESIAN_POINT ( 'NONE',  ( 0.000000000000000000, 0.000000000000000000, -0.3080913168122742518 ) ) ;
#11018 = EDGE_CURVE ( 'NONE', #11392, #560, #200, .T. ) ;
#11019 = EDGE_LOOP ( 'NONE', ( #9260, #9611, #10858 ) ) ;
#11020 = DIRECTION ( 'NONE',  ( -0.5000000000000051070, 0.000000000000000000, 0.8660254037844355990 ) ) ;
#11021 = CARTESIAN_POINT ( 'NONE',  ( 2.500000000000000000, 1.178949249685212974, -2.042000000000001148 ) ) ;
#11022 = ORIENTED_EDGE ( 'NONE', *, *, #9423, .F. ) ;
#11023 = ORIENTED_EDGE ( 'NONE', *, *, #13557, .T. ) ;
#11024 = DIRECTION ( 'NONE',  ( 0.000000000000000000, 0.000000000000000000, 1.000000000000000000 ) ) ;
#11025 = CIRCLE ( 'NONE', #13764, 23.50000000000000355 ) ;
#11026 = ORIENTED_EDGE ( 'NONE', *, *, #7119, .F. ) ;
#11027 = DIRECTION ( 'NONE',  ( 0.000000000000000000, 0.000000000000000000, -1.000000000000000000 ) ) ;
#11028 = CIRCLE ( 'NONE', #7080, 28.00000000000000355 ) ;
#11029 = DIRECTION ( 'NONE',  ( 0.000000000000000000, -0.3090169943749349057, -0.9510565162951576390 ) ) ;
#11030 = AXIS2_PLACEMENT_3D ( 'NONE', #10013, #4480, #197 ) ;
#11031 = EDGE_CURVE ( 'NONE', #3688, #3160, #6585, .T. ) ;
#11032 = ORIENTED_EDGE ( 'NONE', *, *, #16874, .F. ) ;
#11033 = ADVANCED_FACE ( 'NONE', ( #12890 ), #6981, .T. ) ;
#11034 = CIRCLE ( 'NONE', #15303, 12.00000000001200462 ) ;
#11035 = VERTEX_POINT ( 'NONE', #15837 ) ;
#11036 = CARTESIAN_POINT ( 'NONE',  ( 10.00000000000000000, 4.381479206523443359, -32.70783759231081689 ) ) ;
#11037 = AXIS2_PLACEMENT_3D ( 'NONE', #9140, #12367, #7700 ) ;
#11038 = LINE ( 'NONE', #10945, #6963 ) ;
#11039 = CARTESIAN_POINT ( 'NONE',  ( 0.000000000000000000, -24.33982105418938602, 50.71018745830434682 ) ) ;
#11040 = DIRECTION ( 'NONE',  ( 0.000000000000000000, 0.000000000000000000, 1.000000000000000000 ) ) ;
#11041 = FACE_OUTER_BOUND ( 'NONE', #8249, .T. ) ;
#11042 = CARTESIAN_POINT ( 'NONE',  ( 10.00000000000000000, 26.49895292618005271, 49.76630880786320432 ) ) ;
#11043 = CARTESIAN_POINT ( 'NONE',  ( 3.061616997868383043E-15, 15.00000000000000000, -25.00000000000000000 ) ) ;
#11044 = EDGE_LOOP ( 'NONE', ( #16078, #2763, #2653, #17554 ) ) ;
#11045 = CARTESIAN_POINT ( 'NONE',  ( 10.00000000000000000, -50.71018745830427576, -24.33982105418956010 ) ) ;
#11046 = CARTESIAN_POINT ( 'NONE',  ( 0.000000000000000000, 55.74967257055894265, -7.478235706488370660 ) ) ;
#11047 = CARTESIAN_POINT ( 'NONE',  ( -117.1020693116508085, -30.00000000000000000, 19.69080595179778115 ) ) ;
#11048 = CIRCLE ( 'NONE', #2850, 56.24900000005624889 ) ;
#11049 = ORIENTED_EDGE ( 'NONE', *, *, #880, .F. ) ;
#11050 = VERTEX_POINT ( 'NONE', #1181 ) ;
#11051 = ORIENTED_EDGE ( 'NONE', *, *, #17061, .F. ) ;
#11052 = CARTESIAN_POINT ( 'NONE',  ( 10.00000000000000000, 53.06836994729258805, -18.64666490672316712 ) ) ;
#11053 = DIRECTION ( 'NONE',  ( -1.000000000000000000, -0.000000000000000000, 0.000000000000000000 ) ) ;
#11054 = CARTESIAN_POINT ( 'NONE',  ( 10.00000000000000000, 55.33199130079800199, -10.11537145609316646 ) ) ;
#11055 = DIRECTION ( 'NONE',  ( 0.000000000000000000, 0.8910065241883690090, -0.4539904997395448616 ) ) ;
#11056 = DIRECTION ( 'NONE',  ( 0.000000000000000000, 0.000000000000000000, 1.000000000000000000 ) ) ;
#11057 = AXIS2_PLACEMENT_3D ( 'NONE', #12704, #5175, #13943 ) ;
#11058 = DIRECTION ( 'NONE',  ( 0.000000000000000000, 0.000000000000000000, 1.000000000000000000 ) ) ;
#11059 = FACE_OUTER_BOUND ( 'NONE', #2396, .T. ) ;
#11060 = DIRECTION ( 'NONE',  ( 0.000000000000000000, -1.000000000000000000, 0.000000000000000000 ) ) ;
#11061 = ORIENTED_EDGE ( 'NONE', *, *, #17486, .T. ) ;
#11062 = DIRECTION ( 'NONE',  ( -1.000000000000000000, -0.000000000000000000, 0.000000000000000000 ) ) ;
#11063 = ORIENTED_EDGE ( 'NONE', *, *, #9882, .T. ) ;
#11064 = DIRECTION ( 'NONE',  ( -1.000000000000000000, 0.000000000000000000, 0.000000000000000000 ) ) ;
#11065 = DIRECTION ( 'NONE',  ( 0.000000000000000000, 0.000000000000000000, 1.000000000000000000 ) ) ;
#11066 = ORIENTED_EDGE ( 'NONE', *, *, #9578, .F. ) ;
#11067 = EDGE_LOOP ( 'NONE', ( #12757, #2128, #1185, #13218 ) ) ;
#11068 = EDGE_CURVE ( 'NONE', #16413, #17793, #11355, .T. ) ;
#11069 = DIRECTION ( 'NONE',  ( -1.000000000000000000, -0.000000000000000000, 0.000000000000000000 ) ) ;
#11070 = DIRECTION ( 'NONE',  ( 5.947732665067333298E-17, -1.000000000000000000, 5.040995934794347326E-17 ) ) ;
#11072 = EDGE_CURVE ( 'NONE', #14211, #3221, #11129, .T. ) ;
#11071 = DIRECTION ( 'NONE',  ( 0.000000000000000000, 0.3090169943749411785, 0.9510565162951556406 ) ) ;
#11073 = EDGE_LOOP ( 'NONE', ( #13737, #10914, #4408, #8254 ) ) ;
#11074 =( GEOMETRIC_REPRESENTATION_CONTEXT ( 3 ) GLOBAL_UNCERTAINTY_ASSIGNED_CONTEXT ( ( #9785 ) ) GLOBAL_UNIT_ASSIGNED_CONTEXT ( ( #85, #3036, #3122 ) ) REPRESENTATION_CONTEXT ( 'NONE', 'WORKASPACE' ) );
#11075 = PRODUCT_RELATED_PRODUCT_CATEGORY ( 'part', '', ( #9377 ) ) ;
#11076 = ADVANCED_FACE ( 'NONE', ( #8224 ), #7066, .T. ) ;
#11077 = CARTESIAN_POINT ( 'NONE',  ( 0.000000000000000000, -33.95787273855277988, 45.00825343885009033 ) ) ;
#11078 = FACE_OUTER_BOUND ( 'NONE', #15297, .T. ) ;
#11079 = DIRECTION ( 'NONE',  ( -1.000000000000000000, -0.000000000000000000, -0.000000000000000000 ) ) ;
#11080 = CYLINDRICAL_SURFACE ( 'NONE', #3084, 56.24900000005625600 ) ;
#11081 = ADVANCED_FACE ( 'NONE', ( #6785 ), #4223, .T. ) ;
#11082 = ORIENTED_EDGE ( 'NONE', *, *, #7256, .F. ) ;
#11083 = UNCERTAINTY_MEASURE_WITH_UNIT (LENGTH_MEASURE( 1.000000000000000082E-05 ), #16851, 'distance_accuracy_value', 'NONE');
#11084 = CARTESIAN_POINT ( 'NONE',  ( -10.00000000000000000, -42.79754323328189969, -13.90576474687263264 ) ) ;
#11085 = VERTEX_POINT ( 'NONE', #18503 ) ;
#11086 = AXIS2_PLACEMENT_3D ( 'NONE', #13482, #424, #16611 ) ;
#11087 = DIRECTION ( 'NONE',  ( 0.000000000000000000, 0.000000000000000000, 1.000000000000000000 ) ) ;
#11088 = DIRECTION ( 'NONE',  ( -1.000000000000000000, 0.000000000000000000, -0.000000000000000000 ) ) ;
#11089 = LINE ( 'NONE', #14146, #11555 ) ;
#11090 = ORIENTED_EDGE ( 'NONE', *, *, #18422, .F. ) ;
#11091 = AXIS2_PLACEMENT_3D ( 'NONE', #3604, #9118, #14935 ) ;
#11092 = ORIENTED_EDGE ( 'NONE', *, *, #14885, .F. ) ;
#11093 = VECTOR ( 'NONE', #12548, 1000.000000000000000 ) ;
#11094 = EDGE_CURVE ( 'NONE', #12056, #12567, #3842, .T. ) ;
#11095 = DIRECTION ( 'NONE',  ( 0.000000000000000000, 0.000000000000000000, 1.000000000000000000 ) ) ;
#11096 = SURFACE_STYLE_USAGE ( .BOTH. , #8444 ) ;
#11097 = EDGE_CURVE ( 'NONE', #12396, #13512, #12375, .T. ) ;
#11098 = VERTEX_POINT ( 'NONE', #5254 ) ;
#11099 = DIRECTION ( 'NONE',  ( -1.000000000000000000, 0.000000000000000000, 0.000000000000000000 ) ) ;
#11100 = EDGE_CURVE ( 'NONE', #6434, #7434, #9307, .T. ) ;
#11101 = EDGE_CURVE ( 'NONE', #478, #5108, #18742, .T. ) ;
#11102 = CIRCLE ( 'NONE', #1985, 26.24900000002624978 ) ;
#11103 = DIRECTION ( 'NONE',  ( 1.000000000000000000, 0.000000000000000000, 0.000000000000000000 ) ) ;
#11104 = AXIS2_PLACEMENT_3D ( 'NONE', #12147, #2053, #11862 ) ;
#11106 = AXIS2_PLACEMENT_3D ( 'NONE', #3836, #15352, #8125 ) ;
#11105 = PLANE ( 'NONE',  #3260 ) ;
#11107 = ORIENTED_EDGE ( 'NONE', *, *, #16689, .F. ) ;
#11108 = CARTESIAN_POINT ( 'NONE',  ( -0.6666666666666666297, -4.233901974057276973, -3.300726591567087365 ) ) ;
#11109 = ORIENTED_EDGE ( 'NONE', *, *, #53, .F. ) ;
#11110 = CARTESIAN_POINT ( 'NONE',  ( 10.00000000000000000, 0.000000000000000000, 0.000000000000000000 ) ) ;
#11111 = CARTESIAN_POINT ( 'NONE',  ( -0.3562533529037968383, 11.24999999999999467, 23.49729949480461499 ) ) ;
#11112 = CARTESIAN_POINT ( 'NONE',  ( 0.000000000000000000, 0.000000000000000000, 0.000000000000000000 ) ) ;
#11113 = EDGE_LOOP ( 'NONE', ( #11339, #13768, #1247, #15161 ) ) ;
#11114 = CARTESIAN_POINT ( 'NONE',  ( 10.00000000000000000, -15.61693798565454827, -61.03368945066451090 ) ) ;
#11115 = ORIENTED_EDGE ( 'NONE', *, *, #4458, .T. ) ;
#11116 = CARTESIAN_POINT ( 'NONE',  ( 10.04305231718605285, -30.00000000000000000, -28.25933677959240953 ) ) ;
#11117 = CARTESIAN_POINT ( 'NONE',  ( 10.00000000000000000, -31.97297851452390915, -46.27827401617439307 ) ) ;
#11118 = AXIS2_PLACEMENT_3D ( 'NONE', #16633, #18343, #6638 ) ;
#11119 = ORIENTED_EDGE ( 'NONE', *, *, #5319, .F. ) ;
#11120 = ORIENTED_EDGE ( 'NONE', *, *, #9354, .F. ) ;
#11121 = VERTEX_POINT ( 'NONE', #29 ) ;
#11122 = DIRECTION ( 'NONE',  ( 0.000000000000000000, 1.000000000000000000, 0.000000000000000000 ) ) ;
#11123 = FACE_OUTER_BOUND ( 'NONE', #13799, .T. ) ;
#11124 = CIRCLE ( 'NONE', #18745, 24.00000000002399858 ) ;
#11125 = VECTOR ( 'NONE', #18098, 1000.000000000000000 ) ;
#11126 = EDGE_CURVE ( 'NONE', #10711, #15712, #2876, .T. ) ;
#11127 = AXIS2_PLACEMENT_3D ( 'NONE', #15473, #11069, #9370 ) ;
#11128 = VERTEX_POINT ( 'NONE', #4672 ) ;
#11129 = CIRCLE ( 'NONE', #18136, 7.500000000000007105 ) ;
#11130 = AXIS2_PLACEMENT_3D ( 'NONE', #45, #1473, #5842 ) ;
#11131 = ORIENTED_EDGE ( 'NONE', *, *, #71, .T. ) ;
#11132 = DIRECTION ( 'NONE',  ( -1.000000000000000000, 0.000000000000000000, 0.000000000000000000 ) ) ;
#11133 = AXIS2_PLACEMENT_3D ( 'NONE', #6352, #7668, #13496 ) ;
#11134 = DIRECTION ( 'NONE',  ( 0.9998647328874151752, -0.01644736842105263067, 0.000000000000000000 ) ) ;
#11135 = AXIS2_PLACEMENT_3D ( 'NONE', #17897, #11980, #6272 ) ;
#11136 = DIRECTION ( 'NONE',  ( -1.000000000000000000, -0.000000000000000000, -0.000000000000000000 ) ) ;
#11137 = PLANE ( 'NONE',  #16315 ) ;
#11138 = LINE ( 'NONE', #8294, #14254 ) ;
#11139 = CYLINDRICAL_SURFACE ( 'NONE', #4924, 63.00000000006298961 ) ;
#11140 = LINE ( 'NONE', #11246, #1703 ) ;
#11141 = ORIENTED_EDGE ( 'NONE', *, *, #14365, .T. ) ;
#11142 = CARTESIAN_POINT ( 'NONE',  ( 0.1756481739660539498, -4.720212674038995360, -3.469390959564070620 ) ) ;
#11143 = DIRECTION ( 'NONE',  ( -1.000000000000000000, -0.000000000000000000, -0.000000000000000000 ) ) ;
#11144 = DIRECTION ( 'NONE',  ( 0.000000000000000000, -1.000000000000000000, -1.040834085585042960E-14 ) ) ;
#11145 = LINE ( 'NONE', #4211, #18334 ) ;
#11146 = AXIS2_PLACEMENT_3D ( 'NONE', #7225, #7320, #8477 ) ;
#11147 = AXIS2_PLACEMENT_3D ( 'NONE', #7897, #12273, #15142 ) ;
#11148 = AXIS2_PLACEMENT_3D ( 'NONE', #5325, #5441, #17069 ) ;
#11149 = ORIENTED_EDGE ( 'NONE', *, *, #5790, .F. ) ;
#11150 = AXIS2_PLACEMENT_3D ( 'NONE', #9736, #7827, #13651 ) ;
#11151 = CIRCLE ( 'NONE', #14813, 2.396904916527699214 ) ;
#11152 = EDGE_CURVE ( 'NONE', #4158, #12684, #2014, .T. ) ;
#11153 = ORIENTED_EDGE ( 'NONE', *, *, #15569, .T. ) ;
#11154 = ORIENTED_EDGE ( 'NONE', *, *, #2608, .T. ) ;
#11155 = DIRECTION ( 'NONE',  ( -1.000000000000000000, 0.000000000000000000, 0.000000000000000000 ) ) ;
#11156 = PRESENTATION_STYLE_ASSIGNMENT (( #8313 ) ) ;
#11157 = CIRCLE ( 'NONE', #13010, 4.000000000000000000 ) ;
#11158 = DIRECTION ( 'NONE',  ( 0.000000000000000000, -0.8910065241883722287, 0.4539904997395383113 ) ) ;
#11159 = CARTESIAN_POINT ( 'NONE',  ( 10.04305231718579705, -26.50000000000000000, 30.90933677959249337 ) ) ;
#11160 = CARTESIAN_POINT ( 'NONE',  ( 10.00000000000000000, 55.74967257055883607, 7.478235706489176238 ) ) ;
#11161 = DIRECTION ( 'NONE',  ( 1.000000000000000000, 0.000000000000000000, 0.000000000000000000 ) ) ;
#11162 = CARTESIAN_POINT ( 'NONE',  ( 10.00000000000000000, -7.813799127873676476, 55.83748330407405547 ) ) ;
#11163 = VECTOR ( 'NONE', #16835, 1000.000000000000000 ) ;
#11164 = DIRECTION ( 'NONE',  ( -1.000000000000000000, 0.000000000000000000, 0.000000000000000000 ) ) ;
#11165 = ORIENTED_EDGE ( 'NONE', *, *, #1801, .T. ) ;
#11166 = CIRCLE ( 'NONE', #5399, 63.00000000006298961 ) ;
#11167 = DIRECTION ( 'NONE',  ( 0.000000000000000000, 1.000000000000000000, 0.000000000000000000 ) ) ;
#11168 = ORIENTED_EDGE ( 'NONE', *, *, #13242, .T. ) ;
#11169 = EDGE_CURVE ( 'NONE', #4173, #18122, #14789, .T. ) ;
#11170 = DIRECTION ( 'NONE',  ( -0.000000000000000000, 0.8660254037844392627, 0.4999999999999990008 ) ) ;
#11171 = CARTESIAN_POINT ( 'NONE',  ( -11.25000000000000355, 0.000000000000000000, -28.00000000000000355 ) ) ;
#11172 = ORIENTED_EDGE ( 'NONE', *, *, #4575, .F. ) ;
#11173 = ORIENTED_EDGE ( 'NONE', *, *, #15650, .F. ) ;
#11174 = FACE_OUTER_BOUND ( 'NONE', #4417, .T. ) ;
#11175 = DIRECTION ( 'NONE',  ( 6.123233995736766036E-17, -1.000000000000000000, 0.000000000000000000 ) ) ;
#11176 = ADVANCED_FACE ( 'NONE', ( #1541 ), #12664, .T. ) ;
#11177 = CARTESIAN_POINT ( 'NONE',  ( 10.00000000000000000, 24.46385708179996854, -9.514709542736643044 ) ) ;
#11178 = VERTEX_POINT ( 'NONE', #7429 ) ;
#11179 = CONICAL_SURFACE ( 'NONE', #16363, 2.041999999999999815, 1.047197551196591858 ) ;
#11180 = VECTOR ( 'NONE', #14325, 1000.000000000000000 ) ;
#11181 = VECTOR ( 'NONE', #5379, 1000.000000000000000 ) ;
#11182 = VECTOR ( 'NONE', #14115, 1000.000000000000000 ) ;
#11183 = LINE ( 'NONE', #5276, #4424 ) ;
#11184 = CARTESIAN_POINT ( 'NONE',  ( 13.90576474687263264, 0.000000000000000000, -42.79754323328189969 ) ) ;
#11185 = CARTESIAN_POINT ( 'NONE',  ( 10.00000000000000000, 6.681932690256967788, 25.38428207620324883 ) ) ;
#11186 = CYLINDRICAL_SURFACE ( 'NONE', #8530, 63.00000000006298961 ) ;
#11187 = EDGE_CURVE ( 'NONE', #3106, #5418, #6104, .T. ) ;
#11188 = AXIS2_PLACEMENT_3D ( 'NONE', #10802, #3681, #9766 ) ;
#11189 = CARTESIAN_POINT ( 'NONE',  ( 0.000000000000000000, 58.55669782892461939, 23.24033432160458545 ) ) ;
#11190 = ORIENTED_EDGE ( 'NONE', *, *, #6989, .F. ) ;
#11191 = AXIS2_PLACEMENT_3D ( 'NONE', #487, #16126, #8871 ) ;
#11192 = CARTESIAN_POINT ( 'NONE',  ( 10.00000000000000000, -38.81885513160016643, 40.70683587897944022 ) ) ;
#11193 = CARTESIAN_POINT ( 'NONE',  ( 10.00000000000000000, 0.000000000000000000, 0.000000000000000000 ) ) ;
#11194 = CARTESIAN_POINT ( 'NONE',  ( 10.00000000000000000, 5.876895005583349985, -62.72529079327799906 ) ) ;
#11195 = AXIS2_PLACEMENT_3D ( 'NONE', #9164, #14787, #16416 ) ;
#11196 = EDGE_LOOP ( 'NONE', ( #4903, #613, #2918, #18591 ) ) ;
#11197 = VERTEX_POINT ( 'NONE', #1627 ) ;
#11198 = CIRCLE ( 'NONE', #13637, 26.24900000002624978 ) ;
#11199 = APPLICATION_CONTEXT ( 'automotive_design' ) ;
#11200 = CARTESIAN_POINT ( 'NONE',  ( 0.000000000000000000, -46.27827401617379621, -31.97297851452475470 ) ) ;
#11201 =( NAMED_UNIT ( * ) PLANE_ANGLE_UNIT ( ) SI_UNIT ( $, .RADIAN. ) );
#11202 = VERTEX_POINT ( 'NONE', #17539 ) ;
#11203 = DIRECTION ( 'NONE',  ( -1.000000000000000000, -0.000000000000000000, -0.000000000000000000 ) ) ;
#11204 = AXIS2_PLACEMENT_3D ( 'NONE', #15188, #16710, #13748 ) ;
#11205 = CIRCLE ( 'NONE', #4235, 56.24900000005625600 ) ;
#11206 = DIRECTION ( 'NONE',  ( 0.000000000000000000, -0.8090169943749532244, 0.5877852522924652545 ) ) ;
#11207 = AXIS2_PLACEMENT_3D ( 'NONE', #984, #6873, #3652 ) ;
#11208 = VECTOR ( 'NONE', #6834, 1000.000000000000000 ) ;
#11209 = DIRECTION ( 'NONE',  ( 0.000000000000000000, 0.5877852522924741363, -0.8090169943749465631 ) ) ;
#11210 = EDGE_CURVE ( 'NONE', #7022, #15970, #7625, .T. ) ;
#11211 = ORIENTED_EDGE ( 'NONE', *, *, #17189, .T. ) ;
#11212 = ADVANCED_FACE ( 'NONE', ( #5826 ), #14676, .T. ) ;
#11213 = DIRECTION ( 'NONE',  ( 0.9938152567191714803, 0.000000000000000000, -0.1110460963393456596 ) ) ;
#11214 = EDGE_CURVE ( 'NONE', #4499, #7671, #16292, .T. ) ;
#11215 = ORIENTED_EDGE ( 'NONE', *, *, #5400, .F. ) ;
#11216 = DIRECTION ( 'NONE',  ( 0.000000000000000000, 0.000000000000000000, 1.000000000000000000 ) ) ;
#11217 = CARTESIAN_POINT ( 'NONE',  ( 10.00000000000000000, -6.681932690257146312, 25.38428207620320620 ) ) ;
#11218 = DIRECTION ( 'NONE',  ( -0.000000000000000000, 1.000000000000000000, 0.000000000000000000 ) ) ;
#11219 = ORIENTED_EDGE ( 'NONE', *, *, #16677, .T. ) ;
#11220 = CARTESIAN_POINT ( 'NONE',  ( 5.000000000000000000, -54.20017844242489247, -32.11449294037253566 ) ) ;
#11221 = ORIENTED_EDGE ( 'NONE', *, *, #18275, .T. ) ;
#11222 = EDGE_CURVE ( 'NONE', #14229, #2916, #8701, .T. ) ;
#11223 = CARTESIAN_POINT ( 'NONE',  ( 10.00000000000000000, 0.000000000000000000, 0.000000000000000000 ) ) ;
#11224 = CARTESIAN_POINT ( 'NONE',  ( -10.00000000000000000, 0.000000000000000000, 0.000000000000000000 ) ) ;
#11225 = VECTOR ( 'NONE', #5172, 1000.000000000000000 ) ;
#11226 = VERTEX_POINT ( 'NONE', #1718 ) ;
#11227 = ORIENTED_EDGE ( 'NONE', *, *, #4822, .F. ) ;
#11228 = LINE ( 'NONE', #6750, #17208 ) ;
#11229 = AXIS2_PLACEMENT_3D ( 'NONE', #11878, #8737, #4640 ) ;
#11230 = ORIENTED_EDGE ( 'NONE', *, *, #12997, .T. ) ;
#11231 = CARTESIAN_POINT ( 'NONE',  ( 0.000000000000000000, 0.000000000000000000, 0.000000000000000000 ) ) ;
#11232 = DIRECTION ( 'NONE',  ( 0.000000000000000000, 0.000000000000000000, -1.000000000000000000 ) ) ;
#11233 = AXIS2_PLACEMENT_3D ( 'NONE', #2922, #5513, #17408 ) ;
#11234 = ADVANCED_FACE ( 'NONE', ( #10117, #7341, #9050, #1819, #14489, #15924, #11639 ), #13250, .F. ) ;
#11235 = CIRCLE ( 'NONE', #7574, 24.00000000002400213 ) ;
#11236 = ORIENTED_EDGE ( 'NONE', *, *, #9594, .T. ) ;
#11237 = EDGE_CURVE ( 'NONE', #2561, #11050, #4450, .T. ) ;
#11238 = AXIS2_PLACEMENT_3D ( 'NONE', #11388, #18541, #2732 ) ;
#11239 = ORIENTED_EDGE ( 'NONE', *, *, #8452, .F. ) ;
#11240 = DIRECTION ( 'NONE',  ( -0.000000000000000000, 1.000000000000000000, -0.000000000000000000 ) ) ;
#11241 = LINE ( 'NONE', #8653, #8384 ) ;
#11242 = LINE ( 'NONE', #11421, #4760 ) ;
#11243 = CARTESIAN_POINT ( 'NONE',  ( 10.00000000000000000, 40.19788616105679324, -48.50907078259339755 ) ) ;
#11244 = DIRECTION ( 'NONE',  ( 1.000000000000000000, 0.000000000000000000, 0.000000000000000000 ) ) ;
#11245 = CARTESIAN_POINT ( 'NONE',  ( 5.000000000000000000, -32.46095361140696411, 5.940243314904090077 ) ) ;
#11246 = CARTESIAN_POINT ( 'NONE',  ( -90.72413394419160682, -14.11572627500821042, 4.947285117213269245 ) ) ;
#11247 = VERTEX_POINT ( 'NONE', #4395 ) ;
#11248 = CARTESIAN_POINT ( 'NONE',  ( 10.00000000000000000, 5.086963483077203918, 27.72801475327284138 ) ) ;
#11249 = EDGE_CURVE ( 'NONE', #6793, #3669, #8715, .T. ) ;
#11250 = FACE_OUTER_BOUND ( 'NONE', #1529, .T. ) ;
#11251 = DIRECTION ( 'NONE',  ( 0.000000000000000000, 0.000000000000000000, 1.000000000000000000 ) ) ;
#11252 = AXIS2_PLACEMENT_3D ( 'NONE', #9726, #18485, #18584 ) ;
#11253 = CARTESIAN_POINT ( 'NONE',  ( 10.00000000000000000, 40.70683587898012235, -38.81885513159945589 ) ) ;
#11254 = CONTEXT_DEPENDENT_SHAPE_REPRESENTATION ( #18524, #13018 ) ;
#11255 = AXIS2_PLACEMENT_3D ( 'NONE', #17197, #17739, #10222 ) ;
#11256 = ORIENTED_EDGE ( 'NONE', *, *, #16856, .F. ) ;
#11257 = VERTEX_POINT ( 'NONE', #5911 ) ;
#11258 = VERTEX_POINT ( 'NONE', #16016 ) ;
#11259 = CARTESIAN_POINT ( 'NONE',  ( 10.00000000000000000, 14.19907017806900207, -22.07705612348824076 ) ) ;
#11260 = CARTESIAN_POINT ( 'NONE',  ( 0.000000000000000000, 0.000000000000000000, 0.000000000000000000 ) ) ;
#11261 = VECTOR ( 'NONE', #10495, 1000.000000000000000 ) ;
#11262 = FILL_AREA_STYLE ('',( #118 ) ) ;
#11263 = CARTESIAN_POINT ( 'NONE',  ( 4.000000000000000000, 0.000000000000000000, 0.000000000000000000 ) ) ;
#11264 = AXIS2_PLACEMENT_3D ( 'NONE', #15550, #6978, #5348 ) ;
#11265 = CYLINDRICAL_SURFACE ( 'NONE', #3266, 33.00000000003299760 ) ;
#11266 = CARTESIAN_POINT ( 'NONE',  ( 0.000000000000000000, 0.000000000000000000, 0.000000000000000000 ) ) ;
#11267 = DIRECTION ( 'NONE',  ( -1.000000000000000000, -0.000000000000000000, -0.000000000000000000 ) ) ;
#11268 = CARTESIAN_POINT ( 'NONE',  ( 4.000000000000000000, 0.000000000000000000, 0.000000000000000000 ) ) ;
#11269 = ORIENTED_EDGE ( 'NONE', *, *, #2408, .F. ) ;
#11270 = CYLINDRICAL_SURFACE ( 'NONE', #16085, 0.7500000000000000000 ) ;
#11271 = VERTEX_POINT ( 'NONE', #16204 ) ;
#11272 = EDGE_CURVE ( 'NONE', #17009, #4564, #8778, .T. ) ;
#11273 = CARTESIAN_POINT ( 'NONE',  ( 10.04305231718579705, -30.00000000000000000, 30.90933677959249337 ) ) ;
#11274 = CARTESIAN_POINT ( 'NONE',  ( 10.00000000000000000, 40.58063702438344933, 39.14194549634378006 ) ) ;
#11275 = ORIENTED_EDGE ( 'NONE', *, *, #16440, .F. ) ;
#11276 = LINE ( 'NONE', #17097, #17818 ) ;
#11277 = DIRECTION ( 'NONE',  ( 6.123233995736766036E-17, -1.000000000000000000, 0.000000000000000000 ) ) ;
#11278 = FACE_OUTER_BOUND ( 'NONE', #14557, .T. ) ;
#11279 = ORIENTED_EDGE ( 'NONE', *, *, #11793, .T. ) ;
#11280 = EDGE_CURVE ( 'NONE', #2724, #16979, #16114, .T. ) ;
#11281 = DIRECTION ( 'NONE',  ( -1.000000000000000000, -0.000000000000000000, -0.000000000000000000 ) ) ;
#11282 = DIRECTION ( 'NONE',  ( -1.000000000000000000, 0.000000000000000000, -0.000000000000000000 ) ) ;
#11283 = CARTESIAN_POINT ( 'NONE',  ( 10.00000000000000000, 22.07705612348859958, -14.19907017806844252 ) ) ;
#11284 = DIRECTION ( 'NONE',  ( 1.000000000000000000, 0.000000000000000000, 0.000000000000000000 ) ) ;
#11285 = EDGE_CURVE ( 'NONE', #38, #5250, #3257, .T. ) ;
#11286 = CARTESIAN_POINT ( 'NONE',  ( 0.000000000000000000, 20.41355805489643060, -19.44239304137353841 ) ) ;
#11287 = EDGE_LOOP ( 'NONE', ( #671, #3042, #10369, #8807 ) ) ;
#11288 = VECTOR ( 'NONE', #15483, 1000.000000000000000 ) ;
#11289 = DIRECTION ( 'NONE',  ( 0.000000000000000000, 0.000000000000000000, 1.000000000000000000 ) ) ;
#11290 = DIRECTION ( 'NONE',  ( 0.000000000000000000, 0.000000000000000000, -1.000000000000000000 ) ) ;
#11291 = DIRECTION ( 'NONE',  ( 0.000000000000000000, 1.000000000000000000, 0.000000000000000000 ) ) ;
#11292 = ORIENTED_EDGE ( 'NONE', *, *, #6689, .F. ) ;
#11293 = VERTEX_POINT ( 'NONE', #6481 ) ;
#11294 = DIRECTION ( 'NONE',  ( 0.000000000000000000, 0.000000000000000000, 1.000000000000000000 ) ) ;
#11295 = ORIENTED_EDGE ( 'NONE', *, *, #17390, .F. ) ;
#11296 = CARTESIAN_POINT ( 'NONE',  ( 1.836970198721029747E-14, 3.000000000000000000, 150.0000000000000000 ) ) ;
#11297 = CIRCLE ( 'NONE', #649, 1.250000000000001110 ) ;
#11298 = CARTESIAN_POINT ( 'NONE',  ( 10.00000000000000000, 27.94286728106398243, -3.730438010304017116 ) ) ;
#11299 = DIRECTION ( 'NONE',  ( 0.000000000000000000, 0.000000000000000000, 1.000000000000000000 ) ) ;
#11300 = ORIENTED_EDGE ( 'NONE', *, *, #17971, .F. ) ;
#11301 = DIRECTION ( 'NONE',  ( -0.08031988216184954288, 0.000000000000000000, -0.9967691390334607604 ) ) ;
#11302 = VECTOR ( 'NONE', #16400, 1000.000000000000000 ) ;
#11303 = AXIS2_PLACEMENT_3D ( 'NONE', #18278, #5223, #9602 ) ;
#11304 = ORIENTED_EDGE ( 'NONE', *, *, #9953, .F. ) ;
#11306 = DIRECTION ( 'NONE',  ( -1.000000000000000000, 0.000000000000000000, 0.000000000000000000 ) ) ;
#11305 = UNCERTAINTY_MEASURE_WITH_UNIT (LENGTH_MEASURE( 1.000000000000000082E-05 ), #18056, 'distance_accuracy_value', 'NONE');
#11307 = FACE_OUTER_BOUND ( 'NONE', #1950, .T. ) ;
#11308 = DIRECTION ( 'NONE',  ( 0.000000000000000000, 0.000000000000000000, -1.000000000000000000 ) ) ;
#11309 = ORIENTED_EDGE ( 'NONE', *, *, #12199, .T. ) ;
#11310 = CARTESIAN_POINT ( 'NONE',  ( 0.000000000000000000, 55.83748330407397020, 7.813799127874245798 ) ) ;
#11311 = ORIENTED_EDGE ( 'NONE', *, *, #5342, .F. ) ;
#11312 = DIRECTION ( 'NONE',  ( 0.000000000000000000, 0.000000000000000000, 1.000000000000000000 ) ) ;
#11313 = DIRECTION ( 'NONE',  ( -1.000000000000000000, -0.000000000000000000, -0.000000000000000000 ) ) ;
#11314 = ORIENTED_EDGE ( 'NONE', *, *, #9820, .F. ) ;
#11315 = ORIENTED_EDGE ( 'NONE', *, *, #10514, .F. ) ;
#11316 = DIRECTION ( 'NONE',  ( 0.000000000000000000, 0.000000000000000000, 1.000000000000000000 ) ) ;
#11317 =( LENGTH_UNIT ( ) NAMED_UNIT ( * ) SI_UNIT ( .MILLI., .METRE. ) );
#11318 = VERTEX_POINT ( 'NONE', #5040 ) ;
#11319 = LINE ( 'NONE', #4282, #909 ) ;
#11320 = CARTESIAN_POINT ( 'NONE',  ( 0.000000000000000000, 0.000000000000000000, 0.000000000000000000 ) ) ;
#11321 = ADVANCED_FACE ( 'NONE', ( #6289 ), #3724, .T. ) ;
#11322 = AXIS2_PLACEMENT_3D ( 'NONE', #2567, #17250, #12774 ) ;
#11323 = EDGE_CURVE ( 'NONE', #4962, #8010, #13444, .T. ) ;
#11324 = EDGE_CURVE ( 'NONE', #17432, #4065, #7193, .T. ) ;
#11325 = ORIENTED_EDGE ( 'NONE', *, *, #11349, .F. ) ;
#11326 = EDGE_CURVE ( 'NONE', #18145, #9920, #17836, .T. ) ;
#11327 = PRODUCT ( 'circlip for shafts normal_din_Circlip DIN 471 - 50 x 2', 'circlip for shafts normal_din_Circlip DIN 471 - 50 x 2', '', ( #3082 ) ) ;
#11328 = VERTEX_POINT ( 'NONE', #11992 ) ;
#11329 = FACE_OUTER_BOUND ( 'NONE', #18108, .T. ) ;
#11330 = DIRECTION ( 'NONE',  ( 0.000000000000000000, -0.5000000000000009992, -0.8660254037844380415 ) ) ;
#11331 = CARTESIAN_POINT ( 'NONE',  ( 0.000000000000000000, 0.000000000000000000, 0.000000000000000000 ) ) ;
#11332 = CARTESIAN_POINT ( 'NONE',  ( 0.000000000000000000, 55.33199130079785277, 10.11537145609396404 ) ) ;
#11333 = AXIS2_PLACEMENT_3D ( 'NONE', #2364, #11313, #8181 ) ;
#11334 = EDGE_CURVE ( 'NONE', #11318, #18700, #9326, .T. ) ;
#11335 = CYLINDRICAL_SURFACE ( 'NONE', #5730, 24.00000000002400213 ) ;
#11337 = VECTOR ( 'NONE', #6411, 1000.000000000000000 ) ;
#11336 = DIRECTION ( 'NONE',  ( -0.000000000000000000, 1.000000000000000000, -0.000000000000000000 ) ) ;
#11338 = DIRECTION ( 'NONE',  ( 2.031314180040284764E-16, 1.000000000000000000, 1.301042606982601623E-16 ) ) ;
#11339 = ORIENTED_EDGE ( 'NONE', *, *, #13101, .T. ) ;
#11340 =( REPRESENTATION_RELATIONSHIP ('NONE','NONE', #11014, #2517 ) REPRESENTATION_RELATIONSHIP_WITH_TRANSFORMATION ( #8007 )SHAPE_REPRESENTATION_RELATIONSHIP( ) );
#11341 = CARTESIAN_POINT ( 'NONE',  ( 34.55500000000001393, 0.000000000000000000, 0.000000000000000000 ) ) ;
#11342 = CARTESIAN_POINT ( 'NONE',  ( 0.000000000000000000, 0.000000000000000000, -1.000000000000000000 ) ) ;
#11343 = CARTESIAN_POINT ( 'NONE',  ( 0.000000000000000000, 0.000000000000000000, 0.000000000000000000 ) ) ;
#11344 = EDGE_CURVE ( 'NONE', #15878, #11369, #9320, .T. ) ;
#11345 = CONTEXT_DEPENDENT_SHAPE_REPRESENTATION ( #11945, #14528 ) ;
#11346 = EDGE_CURVE ( 'NONE', #6188, #14229, #4758, .T. ) ;
#11347 = VERTEX_POINT ( 'NONE', #17809 ) ;
#11348 = AXIS2_PLACEMENT_3D ( 'NONE', #9769, #1015, #16915 ) ;
#11349 = EDGE_CURVE ( 'NONE', #12355, #13797, #506, .T. ) ;
#11350 = EDGE_CURVE ( 'NONE', #8822, #12311, #12061, .T. ) ;
#11351 = EDGE_LOOP ( 'NONE', ( #13774, #9654, #13138, #6098 ) ) ;
#11352 = CARTESIAN_POINT ( 'NONE',  ( 2.500000000000000000, 2.357898499370431722, -2.818925648462311528E-15 ) ) ;
#11353 = FACE_OUTER_BOUND ( 'NONE', #3882, .T. ) ;
#11354 = ORIENTED_EDGE ( 'NONE', *, *, #13415, .F. ) ;
#11355 = LINE ( 'NONE', #17173, #4743 ) ;
#11356 = CARTESIAN_POINT ( 'NONE',  ( 10.00000000000000000, 0.000000000000000000, 0.000000000000000000 ) ) ;
#11357 = DIRECTION ( 'NONE',  ( -1.000000000000000000, 0.000000000000000000, 0.000000000000000000 ) ) ;
#11358 = CARTESIAN_POINT ( 'NONE',  ( -56.50000000009000445, -34.99999999999999289, -2.649999999999610889 ) ) ;
#11359 = ORIENTED_EDGE ( 'NONE', *, *, #3776, .F. ) ;
#11360 = DIRECTION ( 'NONE',  ( 0.000000000000000000, 0.000000000000000000, 1.000000000000000000 ) ) ;
#11361 = ORIENTED_EDGE ( 'NONE', *, *, #57, .F. ) ;
#11362 = AXIS2_PLACEMENT_3D ( 'NONE', #11273, #5474, #4044 ) ;
#11363 = PLANE ( 'NONE',  #4389 ) ;
#11364 = DIRECTION ( 'NONE',  ( 0.000000000000000000, 1.000000000000000000, 0.000000000000000000 ) ) ;
#11365 = ORIENTED_EDGE ( 'NONE', *, *, #2154, .F. ) ;
#11366 = DIRECTION ( 'NONE',  ( -1.000000000000000000, 0.000000000000000000, 0.000000000000000000 ) ) ;
#11367 = APPLICATION_PROTOCOL_DEFINITION ( 'draft international standard', 'automotive_design', 1998, #15708 ) ;
#11368 = DIRECTION ( 'NONE',  ( 0.000000000000000000, 0.000000000000000000, 1.000000000000000000 ) ) ;
#11369 = VERTEX_POINT ( 'NONE', #15053 ) ;
#11370 = EDGE_CURVE ( 'NONE', #12051, #3115, #5681, .T. ) ;
#11371 = MECHANICAL_DESIGN_GEOMETRIC_PRESENTATION_REPRESENTATION (  '', ( #10161 ), #15028 ) ;
#11372 = CARTESIAN_POINT ( 'NONE',  ( 2.500000000000000000, 2.357898499370432166, -2.385244779468109755E-15 ) ) ;
#11373 = DIRECTION ( 'NONE',  ( -1.000000000000000000, 0.000000000000000000, 0.000000000000000000 ) ) ;
#11374 = DIRECTION ( 'NONE',  ( -1.000000000000000000, -0.000000000000000000, 0.000000000000000000 ) ) ;
#11375 = LINE ( 'NONE', #1103, #4011 ) ;
#11376 = CARTESIAN_POINT ( 'NONE',  ( 13.90576474687299680, 0.000000000000000000, 42.79754323328179311 ) ) ;
#11377 = ORIENTED_EDGE ( 'NONE', *, *, #402, .F. ) ;
#11378 = CARTESIAN_POINT ( 'NONE',  ( 10.00000000000000000, 53.29895248911675765, 18.38754094778260040 ) ) ;
#11379 = CARTESIAN_POINT ( 'NONE',  ( 0.000000000000000000, 7.478235706488965739, 55.74967257055886449 ) ) ;
#11380 = CARTESIAN_POINT ( 'NONE',  ( -10.00000000000000000, 0.000000000000000000, 0.000000000000000000 ) ) ;
#11381 = ORIENTED_EDGE ( 'NONE', *, *, #13995, .T. ) ;
#11382 = ORIENTED_EDGE ( 'NONE', *, *, #15050, .T. ) ;
#11383 = DIRECTION ( 'NONE',  ( 0.000000000000000000, 0.000000000000000000, 1.000000000000000000 ) ) ;
#11384 =( LENGTH_UNIT ( ) NAMED_UNIT ( * ) SI_UNIT ( .MILLI., .METRE. ) );
#11385 = PRESENTATION_LAYER_ASSIGNMENT (  '', '', ( #745 ) ) ;
#11386 = EDGE_CURVE ( 'NONE', #1316, #9138, #5977, .T. ) ;
#11387 = ORIENTED_EDGE ( 'NONE', *, *, #14210, .T. ) ;
#11388 = CARTESIAN_POINT ( 'NONE',  ( 10.00000000000000000, 0.000000000000000000, 0.000000000000000000 ) ) ;
#11389 = EDGE_CURVE ( 'NONE', #4075, #18014, #10756, .T. ) ;
#11390 = FACE_BOUND ( 'NONE', #5786, .T. ) ;
#11391 = CARTESIAN_POINT ( 'NONE',  ( 10.00000000000000000, -3.730438010304114371, -27.94286728106396822 ) ) ;
#11392 = VERTEX_POINT ( 'NONE', #388 ) ;
#11393 = DIRECTION ( 'NONE',  ( 1.000000000000000000, 0.000000000000000000, 0.000000000000000000 ) ) ;
#11394 = ORIENTED_EDGE ( 'NONE', *, *, #3881, .F. ) ;
#11395 = DIRECTION ( 'NONE',  ( -1.000000000000000000, 0.000000000000000000, 0.000000000000000000 ) ) ;
#11396 = DIRECTION ( 'NONE',  ( -1.000000000000000000, 0.000000000000000000, 0.000000000000000000 ) ) ;
#11397 = AXIS2_PLACEMENT_3D ( 'NONE', #16140, #8887, #11754 ) ;
#11398 = ORIENTED_EDGE ( 'NONE', *, *, #5658, .F. ) ;
#11399 = DIRECTION ( 'NONE',  ( -1.000000000000000000, 0.000000000000000000, 0.000000000000000000 ) ) ;
#11400 = ORIENTED_EDGE ( 'NONE', *, *, #13897, .T. ) ;
#11401 = CARTESIAN_POINT ( 'NONE',  ( 10.00000000000000000, 0.000000000000000000, 0.000000000000000000 ) ) ;
#11402 = DIRECTION ( 'NONE',  ( 0.000000000000000000, 0.000000000000000000, 1.000000000000000000 ) ) ;
#11403 = ORIENTED_EDGE ( 'NONE', *, *, #15143, .T. ) ;
#11404 = ORIENTED_EDGE ( 'NONE', *, *, #198, .T. ) ;
#11405 = EDGE_CURVE ( 'NONE', #9233, #858, #2191, .T. ) ;
#11406 = CARTESIAN_POINT ( 'NONE',  ( 11.25000000000000000, 3.306546357697854128E-15, 27.00000000000000355 ) ) ;
#11407 = SURFACE_STYLE_FILL_AREA ( #12850 ) ;
#11408 = ORIENTED_EDGE ( 'NONE', *, *, #4101, .F. ) ;
#11409 = CARTESIAN_POINT ( 'NONE',  ( -23.48826165280197031, 11.24999999999999467, -0.7426739052322692825 ) ) ;
#11410 = DIRECTION ( 'NONE',  ( 0.000000000000000000, -0.5000000000000013323, -0.8660254037844380415 ) ) ;
#11411 = ADVANCED_FACE ( 'NONE', ( #16674 ), #18001, .T. ) ;
#11412 = AXIS2_PLACEMENT_3D ( 'NONE', #2512, #3667, #15474 ) ;
#11413 = AXIS2_PLACEMENT_3D ( 'NONE', #11969, #17778, #10725 ) ;
#11414 = VECTOR ( 'NONE', #15646, 1000.000000000000000 ) ;
#11415 = CARTESIAN_POINT ( 'NONE',  ( 11.25000000000000000, 0.000000000000000000, -27.00000000000000355 ) ) ;
#11416 = ORIENTED_EDGE ( 'NONE', *, *, #7274, .F. ) ;
#11417 = VECTOR ( 'NONE', #3315, 1000.000000000000000 ) ;
#11418 = ORIENTED_EDGE ( 'NONE', *, *, #11423, .T. ) ;
#11419 = DIRECTION ( 'NONE',  ( -0.000000000000000000, 0.000000000000000000, 1.000000000000000000 ) ) ;
#11420 = DIRECTION ( 'NONE',  ( 0.000000000000000000, 0.4539904997395476927, -0.8910065241883673437 ) ) ;
#11421 = CARTESIAN_POINT ( 'NONE',  ( 10.00000000000000000, 20.32630374611208879, -16.60877409751146416 ) ) ;
#11422 = DIRECTION ( 'NONE',  ( 0.000000000000000000, 0.000000000000000000, 1.000000000000000000 ) ) ;
#11423 = EDGE_CURVE ( 'NONE', #3158, #3817, #10839, .T. ) ;
#11424 = EDGE_CURVE ( 'NONE', #13451, #16356, #17259, .T. ) ;
#11425 = LINE ( 'NONE', #7413, #5740 ) ;
#11426 = CARTESIAN_POINT ( 'NONE',  ( -36.40576474687247099, 10.00000000000000000, 26.45033635316149301 ) ) ;
#11427 = AXIS2_PLACEMENT_3D ( 'NONE', #17399, #5589, #11772 ) ;
#11428 = FACE_OUTER_BOUND ( 'NONE', #13148, .T. ) ;
#11429 = ORIENTED_EDGE ( 'NONE', *, *, #13528, .F. ) ;
#11430 = CARTESIAN_POINT ( 'NONE',  ( 0.000000000000000000, 0.000000000000000000, 0.000000000000000000 ) ) ;
#11431 = CIRCLE ( 'NONE', #16588, 2.649999999999999467 ) ;
#11432 = DIRECTION ( 'NONE',  ( 0.000000000000000000, -0.9876883405951393247, 0.1564344650402205161 ) ) ;
#11433 = PRODUCT_RELATED_PRODUCT_CATEGORY ( 'part', '', ( #9207 ) ) ;
#11434 = CYLINDRICAL_SURFACE ( 'NONE', #1480, 4.799999999999999822 ) ;
#11435 = EDGE_LOOP ( 'NONE', ( #7686, #925, #17496, #12400 ) ) ;
#11436 = ORIENTED_EDGE ( 'NONE', *, *, #13957, .T. ) ;
#11437 = CIRCLE ( 'NONE', #3823, 25.00000000000000000 ) ;
#11438 = CIRCLE ( 'NONE', #13866, 2.649999999999992806 ) ;
#11439 = VECTOR ( 'NONE', #15077, 1000.000000000000114 ) ;
#11440 = AXIS2_PLACEMENT_3D ( 'NONE', #8517, #18704, #8695 ) ;
#11441 = VECTOR ( 'NONE', #1778, 1000.000000000000000 ) ;
#11442 = CONICAL_SURFACE ( 'NONE', #10815, 2.041999999999999815, 1.047197551196591858 ) ;
#11443 = EDGE_LOOP ( 'NONE', ( #15917, #8947, #2201, #3825 ) ) ;
#11444 = FACE_OUTER_BOUND ( 'NONE', #1128, .T. ) ;
#11445 = DIRECTION ( 'NONE',  ( 0.000000000000000000, 0.000000000000000000, 1.000000000000000000 ) ) ;
#11446 = ORIENTED_EDGE ( 'NONE', *, *, #2087, .F. ) ;
#11447 = DIRECTION ( 'NONE',  ( 0.000000000000000000, -0.5000000000000013323, -0.8660254037844380415 ) ) ;
#11448 = APPLICATION_CONTEXT ( 'automotive_design' ) ;
#11449 = CARTESIAN_POINT ( 'NONE',  ( 4.000000000000000000, 0.1981133338132474442, 2.382280164152719704E-17 ) ) ;
#11450 = EDGE_CURVE ( 'NONE', #11921, #12688, #2648, .T. ) ;
#11451 = EDGE_CURVE ( 'NONE', #16165, #5694, #13597, .T. ) ;
#11452 = ADVANCED_FACE ( 'NONE', ( #17248, #1053, #8202, #18578, #6762, #5534, #4201 ), #11137, .F. ) ;
#11453 = FACE_OUTER_BOUND ( 'NONE', #10611, .T. ) ;
#11454 = CONICAL_SURFACE ( 'NONE', #2630, 2.055000000000000160, 0.7853981633974794763 ) ;
#11455 = DIRECTION ( 'NONE',  ( -1.000000000000000000, -0.000000000000000000, -0.000000000000000000 ) ) ;
#11456 = VERTEX_POINT ( 'NONE', #8100 ) ;
#11457 = DIRECTION ( 'NONE',  ( -1.000000000000000000, -0.000000000000000000, -0.000000000000000000 ) ) ;
#11458 =( GEOMETRIC_REPRESENTATION_CONTEXT ( 3 ) GLOBAL_UNCERTAINTY_ASSIGNED_CONTEXT ( ( #15111 ) ) GLOBAL_UNIT_ASSIGNED_CONTEXT ( ( #16276, #13431, #12185 ) ) REPRESENTATION_CONTEXT ( 'NONE', 'WORKASPACE' ) );
#11459 = VERTEX_POINT ( 'NONE', #11332 ) ;
#11460 = CIRCLE ( 'NONE', #12040, 24.00000000002399148 ) ;
#11461 = EDGE_CURVE ( 'NONE', #8021, #1435, #13292, .T. ) ;
#11462 = SURFACE_SIDE_STYLE ('',( #5649 ) ) ;
#11463 = CARTESIAN_POINT ( 'NONE',  ( 0.000000000000000000, 0.000000000000000000, 0.000000000000000000 ) ) ;
#11464 = ORIENTED_EDGE ( 'NONE', *, *, #13615, .F. ) ;
#11465 = VECTOR ( 'NONE', #13930, 1000.000000000000000 ) ;
#11466 = B_SPLINE_CURVE_WITH_KNOTS ( 'NONE', 3,
 ( #2136, #7941, #525, #18234, #10891, #8137, #12421, #5182 ),
 .UNSPECIFIED., .F., .F.,
 ( 4, 2, 2, 4 ),
 ( 0.000000000000000000, 0.002450665683189820997, 0.003675998524784731495, 0.004901331366379641993 ),
 .UNSPECIFIED. ) ;
#11467 = CIRCLE ( 'NONE', #3244, 24.00000000002399858 ) ;
#11468 = APPLICATION_PROTOCOL_DEFINITION ( 'draft international standard', 'automotive_design', 1998, #18627 ) ;
#11469 = DIRECTION ( 'NONE',  ( 0.000000000000000000, 1.000000000000000000, 0.000000000000000000 ) ) ;
#11470 = ORIENTED_EDGE ( 'NONE', *, *, #11665, .F. ) ;
#11471 = EDGE_CURVE ( 'NONE', #2470, #890, #5695, .T. ) ;
#11472 = CIRCLE ( 'NONE', #7200, 24.00000000002399858 ) ;
#11473 = AXIS2_PLACEMENT_3D ( 'NONE', #16077, #9985, #11607 ) ;
#11474 = CIRCLE ( 'NONE', #10539, 63.00000000006298961 ) ;
#11475 = FACE_OUTER_BOUND ( 'NONE', #9634, .T. ) ;
#11476 = CYLINDRICAL_SURFACE ( 'NONE', #6383, 24.00000000002400213 ) ;
#11477 = AXIS2_PLACEMENT_3D ( 'NONE', #2635, #1124, #8451 ) ;
#11478 = CIRCLE ( 'NONE', #1443, 24.00000000002400569 ) ;
#11479 = CARTESIAN_POINT ( 'NONE',  ( 10.00000000000000000, -20.41355805489629915, 19.44239304137368407 ) ) ;
#11480 = CARTESIAN_POINT ( 'NONE',  ( 10.00000000000000000, 24.97244012287581683, -57.83923611457293390 ) ) ;
#11481 = EDGE_CURVE ( 'NONE', #12463, #17771, #2671, .T. ) ;
#11482 = CARTESIAN_POINT ( 'NONE',  ( 0.000000000000000000, 12.18267823974788122, -25.42247726998001411 ) ) ;
#11483 = VERTEX_POINT ( 'NONE', #2565 ) ;
#11484 = DIRECTION ( 'NONE',  ( 0.000000000000000000, -0.9510565162951565288, 0.3090169943749382919 ) ) ;
#11485 = LINE ( 'NONE', #13106, #17455 ) ;
#11486 = DIRECTION ( 'NONE',  ( -1.000000000000000000, 0.000000000000000000, -0.000000000000000000 ) ) ;
#11487 = CIRCLE ( 'NONE', #14506, 26.24900000002625333 ) ;
#11488 = EDGE_LOOP ( 'NONE', ( #12537, #14444, #4991, #2976 ) ) ;
#11489 = ORIENTED_EDGE ( 'NONE', *, *, #12257, .F. ) ;
#11490 = EDGE_CURVE ( 'NONE', #3688, #15880, #8110, .T. ) ;
#11491 = CARTESIAN_POINT ( 'NONE',  ( 10.00000000000000000, 50.69000562871642046, 24.68609584167177218 ) ) ;
#11492 = AXIS2_PLACEMENT_3D ( 'NONE', #9695, #17134, #2360 ) ;
#11493 = ORIENTED_EDGE ( 'NONE', *, *, #15543, .F. ) ;
#11494 = AXIS2_PLACEMENT_3D ( 'NONE', #2520, #9855, #15664 ) ;
#11495 = AXIS2_PLACEMENT_3D ( 'NONE', #5465, #13937, #6700 ) ;
#11496 = PRODUCT_DEFINITION_SHAPE ( 'NONE', 'NONE',  #7121 ) ;
#11497 = DIRECTION ( 'NONE',  ( -1.000000000000000000, -0.000000000000000000, -0.000000000000000000 ) ) ;
#11498 = AXIS2_PLACEMENT_3D ( 'NONE', #2358, #9788, #10252 ) ;
#11499 = DIRECTION ( 'NONE',  ( -1.000000000000000000, -0.000000000000000000, 0.000000000000000000 ) ) ;
#11500 = ORIENTED_EDGE ( 'NONE', *, *, #12607, .F. ) ;
#11501 = CARTESIAN_POINT ( 'NONE',  ( 2.500000000000000888, 3.061616997868384127E-16, -4.974599999999998801 ) ) ;
#11502 = AXIS2_PLACEMENT_3D ( 'NONE', #13944, #15359, #10782 ) ;
#11503 = VECTOR ( 'NONE', #7450, 1000.000000000000114 ) ;
#11504 = ORIENTED_EDGE ( 'NONE', *, *, #5854, .F. ) ;
#11505 = CIRCLE ( 'NONE', #3292, 24.00000000002399858 ) ;
#11506 = CARTESIAN_POINT ( 'NONE',  ( -12.69999999999999929, 0.000000000000000000, 0.000000000000000000 ) ) ;
#11507 = EDGE_LOOP ( 'NONE', ( #11528, #8953, #7652, #18540 ) ) ;
#11508 = CYLINDRICAL_SURFACE ( 'NONE', #1386, 24.00000000002399858 ) ;
#11509 = ORIENTED_EDGE ( 'NONE', *, *, #7771, .F. ) ;
#11510 = DIRECTION ( 'NONE',  ( -1.000000000000000000, -0.000000000000000000, -0.000000000000000000 ) ) ;
#11511 = FACE_OUTER_BOUND ( 'NONE', #5593, .T. ) ;
#11512 = ORIENTED_EDGE ( 'NONE', *, *, #5771, .T. ) ;
#11513 = EDGE_LOOP ( 'NONE', ( #15606, #2667, #17668, #11789 ) ) ;
#11514 = EDGE_CURVE ( 'NONE', #18225, #19, #14297, .T. ) ;
#11515 = DIRECTION ( 'NONE',  ( -0.000000000000000000, 1.000000000000000000, -0.000000000000000000 ) ) ;
#11516 = FILL_AREA_STYLE_COLOUR ( '', #7120 ) ;
#11517 = EDGE_LOOP ( 'NONE', ( #16465, #4274 ) ) ;
#11518 = CARTESIAN_POINT ( 'NONE',  ( -4.000000000000000000, -2.309401076758512694, -3.433295621305382461 ) ) ;
#11519 = VECTOR ( 'NONE', #15770, 1000.000000000000000 ) ;
#11520 = CIRCLE ( 'NONE', #13342, 24.00000000002400569 ) ;
#11521 = SHAPE_REPRESENTATION ( 'needle roller bearing_nm_iso_ISO 3030 - 15C5060 - 26,SI,AC,26', ( #8017 ), #16563 ) ;
#11522 = CIRCLE ( 'NONE', #16081, 28.00000000000000711 ) ;
#11523 = AXIS2_PLACEMENT_3D ( 'NONE', #8749, #1426, #11710 ) ;
#11524 = CARTESIAN_POINT ( 'NONE',  ( 4.999999999999999112, 13.79392154159135231, 61.47135697633785156 ) ) ;
#11525 = EDGE_CURVE ( 'NONE', #2085, #2539, #15732, .T. ) ;
#11526 = ORIENTED_EDGE ( 'NONE', *, *, #6057, .T. ) ;
#11527 = AXIS2_PLACEMENT_3D ( 'NONE', #1647, #14701, #7735 ) ;
#11528 = ORIENTED_EDGE ( 'NONE', *, *, #11481, .F. ) ;
#11529 = CARTESIAN_POINT ( 'NONE',  ( 10.00000000000000000, 0.000000000000000000, 0.000000000000000000 ) ) ;
#11530 = FACE_OUTER_BOUND ( 'NONE', #15218, .T. ) ;
#11531 = CARTESIAN_POINT ( 'NONE',  ( 0.000000000000000000, 55.83748330407408389, -7.813799127873475747 ) ) ;
#11532 = CARTESIAN_POINT ( 'NONE',  ( -4.000000000000000000, -2.472261339043343220, -3.687027428081192326 ) ) ;
#11533 = CIRCLE ( 'NONE', #9082, 24.00000000002399858 ) ;
#11534 = EDGE_CURVE ( 'NONE', #6648, #5427, #18458, .T. ) ;
#11535 = DIRECTION ( 'NONE',  ( -1.000000000000000000, -0.000000000000000000, -0.000000000000000000 ) ) ;
#11536 = DIRECTION ( 'NONE',  ( -1.000000000000000000, 0.000000000000000000, 0.000000000000000000 ) ) ;
#11537 = CIRCLE ( 'NONE', #3322, 2.650000000000001243 ) ;
#11538 =( GEOMETRIC_REPRESENTATION_CONTEXT ( 3 ) GLOBAL_UNCERTAINTY_ASSIGNED_CONTEXT ( ( #1953 ) ) GLOBAL_UNIT_ASSIGNED_CONTEXT ( ( #4222, #13527, #10469 ) ) REPRESENTATION_CONTEXT ( 'NONE', 'WORKASPACE' ) );
#11539 = CARTESIAN_POINT ( 'NONE',  ( -90.00000000009001155, 2.081668171172168513E-14, -1.301042606982603940E-15 ) ) ;
#11540 = ORIENTED_EDGE ( 'NONE', *, *, #15276, .T. ) ;
#11541 = AXIS2_PLACEMENT_3D ( 'NONE', #7609, #367, #6174 ) ;
#11542 = DIRECTION ( 'NONE',  ( -1.000000000000000000, 0.000000000000000000, 0.000000000000000000 ) ) ;
#11543 = ORIENTED_EDGE ( 'NONE', *, *, #11187, .F. ) ;
#11544 = DIRECTION ( 'NONE',  ( -1.000000000000000000, -0.000000000000000000, 0.000000000000000000 ) ) ;
#11545 = CYLINDRICAL_SURFACE ( 'NONE', #18654, 5.000000000000000000 ) ;
#11546 = EDGE_LOOP ( 'NONE', ( #955, #3025 ) ) ;
#11547 = VECTOR ( 'NONE', #13168, 1000.000000000000000 ) ;
#11548 = ORIENTED_EDGE ( 'NONE', *, *, #4811, .T. ) ;
#11549 = DIRECTION ( 'NONE',  ( -1.000000000000000000, 0.000000000000000000, 0.000000000000000000 ) ) ;
#11550 = DIRECTION ( 'NONE',  ( 0.000000000000000000, 0.000000000000000000, 1.000000000000000000 ) ) ;
#11551 = VERTEX_POINT ( 'NONE', #878 ) ;
#11552 = SURFACE_SIDE_STYLE ('',( #15740 ) ) ;
#11553 = CARTESIAN_POINT ( 'NONE',  ( -2.500000000000000444, 3.061616997868383634E-16, -25.03750572909317285 ) ) ;
#11554 = CARTESIAN_POINT ( 'NONE',  ( 0.000000000000000000, 0.000000000000000000, -1.500000000000000000 ) ) ;
#11555 = VECTOR ( 'NONE', #1112, 1000.000000000000000 ) ;
#11556 = DIRECTION ( 'NONE',  ( 0.000000000000000000, 0.000000000000000000, 1.000000000000000000 ) ) ;
#11557 = CARTESIAN_POINT ( 'NONE',  ( 10.00000000000000178, 0.000000000000000000, 0.000000000000000000 ) ) ;
#11558 = ORIENTED_EDGE ( 'NONE', *, *, #6641, .T. ) ;
#11559 = CARTESIAN_POINT ( 'NONE',  ( 10.00000000000000000, 13.40641754777665717, 24.79895094899264052 ) ) ;
#11560 = EDGE_LOOP ( 'NONE', ( #14739, #12964, #15771, #10260 ) ) ;
#11561 = VECTOR ( 'NONE', #5498, 1000.000000000000000 ) ;
#11562 =( LENGTH_UNIT ( ) NAMED_UNIT ( * ) SI_UNIT ( .MILLI., .METRE. ) );
#11563 = CARTESIAN_POINT ( 'NONE',  ( 10.00000000000000000, -1.017308535512791767, 56.37237871411032586 ) ) ;
#11564 = ORIENTED_EDGE ( 'NONE', *, *, #6845, .F. ) ;
#11565 = CONTEXT_DEPENDENT_SHAPE_REPRESENTATION ( #6472, #2819 ) ;
#11566 = EDGE_LOOP ( 'NONE', ( #6943, #5227, #3075, #14844 ) ) ;
#11567 = EDGE_CURVE ( 'NONE', #12264, #17712, #4461, .T. ) ;
#11568 = ADVANCED_FACE ( 'NONE', ( #8480 ), #15531, .F. ) ;
#11569 = EDGE_CURVE ( 'NONE', #8684, #1351, #11474, .T. ) ;
#11570 = AXIS2_PLACEMENT_3D ( 'NONE', #6274, #6726, #3425 ) ;
#11571 = VERTEX_POINT ( 'NONE', #11243 ) ;
#11572 = CIRCLE ( 'NONE', #23, 24.00000000002399858 ) ;
#11573 = FACE_BOUND ( 'NONE', #8255, .T. ) ;
#11574 = ADVANCED_FACE ( 'NONE', ( #8290 ), #9945, .T. ) ;
#11575 = CARTESIAN_POINT ( 'NONE',  ( 0.000000000000000000, -25.38428207620317778, -6.681932690257235130 ) ) ;
#11576 = CARTESIAN_POINT ( 'NONE',  ( 0.2500000000000002220, 0.000000000000000000, 0.000000000000000000 ) ) ;
#11577 = CARTESIAN_POINT ( 'NONE',  ( 10.00000000000000000, 50.71018745830443919, 24.33982105418919417 ) ) ;
#11578 = ADVANCED_FACE ( 'NONE', ( #14093 ), #6676, .F. ) ;
#11579 = DIRECTION ( 'NONE',  ( -1.000000000000000000, -0.000000000000000000, -0.000000000000000000 ) ) ;
#11580 = ORIENTED_EDGE ( 'NONE', *, *, #16099, .T. ) ;
#11581 = CARTESIAN_POINT ( 'NONE',  ( 0.000000000000000000, 0.000000000000000000, -0.3080913168122742518 ) ) ;
#11582 = ADVANCED_FACE ( 'NONE', ( #16862 ), #3623, .F. ) ;
#11583 = CARTESIAN_POINT ( 'NONE',  ( 10.00000000000000000, 33.95787273855245303, 45.00825343885033192 ) ) ;
#11584 = LINE ( 'NONE', #14801, #6998 ) ;
#11585 = ORIENTED_EDGE ( 'NONE', *, *, #6399, .F. ) ;
#11586 = ORIENTED_EDGE ( 'NONE', *, *, #12321, .F. ) ;
#11587 = DIRECTION ( 'NONE',  ( -1.000000000000000000, -0.000000000000000000, -0.000000000000000000 ) ) ;
#11588 = COLOUR_RGB ( '',1.000000000000000000, 0.9490196078431372140, 0.9098039215686274384 ) ;
#11589 =( NAMED_UNIT ( * ) PLANE_ANGLE_UNIT ( ) SI_UNIT ( $, .RADIAN. ) );
#11590 = ORIENTED_EDGE ( 'NONE', *, *, #7263, .F. ) ;
#11591 = EDGE_CURVE ( 'NONE', #14348, #13348, #8569, .T. ) ;
#11592 = EDGE_CURVE ( 'NONE', #10140, #11963, #2660, .T. ) ;
#11593 = DIRECTION ( 'NONE',  ( -0.000000000000000000, 1.000000000000000000, -0.000000000000000000 ) ) ;
#11594 = PLANE ( 'NONE',  #16056 ) ;
#11595 = EDGE_CURVE ( 'NONE', #7581, #14103, #10854, .T. ) ;
#11596 = VERTEX_POINT ( 'NONE', #17701 ) ;
#11598 = CIRCLE ( 'NONE', #16456, 24.00000000002399858 ) ;
#11597 = DIRECTION ( 'NONE',  ( -1.000000000000000000, 0.000000000000000000, 0.000000000000000000 ) ) ;
#11599 = ORIENTED_EDGE ( 'NONE', *, *, #8647, .F. ) ;
#11600 = CARTESIAN_POINT ( 'NONE',  ( 0.000000000000000000, 10.11537145609457156, -55.33199130079773909 ) ) ;
#11601 = ORIENTED_EDGE ( 'NONE', *, *, #14021, .F. ) ;
#11602 = ORIENTED_EDGE ( 'NONE', *, *, #1346, .F. ) ;
#11603 = FACE_OUTER_BOUND ( 'NONE', #2725, .T. ) ;
#11604 = CARTESIAN_POINT ( 'NONE',  ( 32.50000000000000000, -26.50000000000000000, 3.680389326632394941E-13 ) ) ;
#11605 = ORIENTED_EDGE ( 'NONE', *, *, #1240, .F. ) ;
#11606 = ORIENTED_EDGE ( 'NONE', *, *, #4817, .T. ) ;
#11607 = DIRECTION ( 'NONE',  ( 0.000000000000000000, 0.000000000000000000, -1.000000000000000000 ) ) ;
#11608 = ORIENTED_EDGE ( 'NONE', *, *, #7642, .F. ) ;
#11609 = CARTESIAN_POINT ( 'NONE',  ( 10.00000000000000000, -33.71303790549235657, -53.22058882792234158 ) ) ;
#11610 = CIRCLE ( 'NONE', #8263, 63.00000000006298961 ) ;
#11611 = DIRECTION ( 'NONE',  ( -1.000000000000000000, 0.000000000000000000, 0.000000000000000000 ) ) ;
#11612 = VECTOR ( 'NONE', #8085, 1000.000000000000000 ) ;
#11613 = EDGE_CURVE ( 'NONE', #16829, #1379, #16351, .T. ) ;
#11614 = EDGE_LOOP ( 'NONE', ( #2886, #3948, #1554, #12994 ) ) ;
#11615 = ORIENTED_EDGE ( 'NONE', *, *, #10744, .T. ) ;
#11616 = CARTESIAN_POINT ( 'NONE',  ( 10.00000000000000000, -20.32630374611172641, -16.60877409751190470 ) ) ;
#11617 = DIRECTION ( 'NONE',  ( 0.000000000000000000, 0.000000000000000000, 1.000000000000000000 ) ) ;
#11618 = DIRECTION ( 'NONE',  ( -0.000000000000000000, 1.000000000000000000, -0.000000000000000000 ) ) ;
#11619 = DIRECTION ( 'NONE',  ( 1.000000000000000000, 0.000000000000000000, 0.000000000000000000 ) ) ;
#11620 = CARTESIAN_POINT ( 'NONE',  ( 0.000000000000000000, -45.00825343884996954, -33.95787273855293620 ) ) ;
#11621 = CARTESIAN_POINT ( 'NONE',  ( 0.000000000000000000, 0.000000000000000000, 0.000000000000000000 ) ) ;
#11622 = DIRECTION ( 'NONE',  ( 1.000000000000000000, 0.000000000000000000, 0.000000000000000000 ) ) ;
#11623 = CARTESIAN_POINT ( 'NONE',  ( 50.00005079999999680, 4.769696007084728073, -1.500000000000000000 ) ) ;
#11624 = ORIENTED_EDGE ( 'NONE', *, *, #9711, .T. ) ;
#11625 = FACE_OUTER_BOUND ( 'NONE', #17241, .T. ) ;
#11626 = DIRECTION ( 'NONE',  ( -1.000000000000000000, -0.000000000000000000, 0.000000000000000000 ) ) ;
#11627 = CIRCLE ( 'NONE', #3409, 24.00000000002399858 ) ;
#11628 = ORIENTED_EDGE ( 'NONE', *, *, #16911, .F. ) ;
#11629 = CARTESIAN_POINT ( 'NONE',  ( 5.000000000000000000, -23.24033432160398860, -58.55669782892485387 ) ) ;
#11630 = DIRECTION ( 'NONE',  ( -1.000000000000000000, -0.000000000000000000, -0.000000000000000000 ) ) ;
#11631 = ADVANCED_FACE ( 'NONE', ( #98 ), #14564, .T. ) ;
#11632 = ADVANCED_FACE ( 'NONE', ( #12951 ), #8748, .T. ) ;
#11633 = VERTEX_POINT ( 'NONE', #7412 ) ;
#11635 = CARTESIAN_POINT ( 'NONE',  ( -12.69999999999999929, 3.306546357697854128E-15, 27.00000000000000355 ) ) ;
#11634 = AXIS2_PLACEMENT_3D ( 'NONE', #16848, #12754, #3795 ) ;
#11636 = DIRECTION ( 'NONE',  ( 1.000000000000000000, 0.000000000000000000, 0.000000000000000000 ) ) ;
#11637 = ORIENTED_EDGE ( 'NONE', *, *, #5680, .T. ) ;
#11638 = CARTESIAN_POINT ( 'NONE',  ( -90.00000000009001155, -88.00000000000000000, -1.301042606982603940E-15 ) ) ;
#11639 = FACE_OUTER_BOUND ( 'NONE', #9827, .T. ) ;
#11640 = CARTESIAN_POINT ( 'NONE',  ( -117.1020693116506379, -30.00000000000000000, -22.34080595179800355 ) ) ;
#11641 = DIRECTION ( 'NONE',  ( 0.000000000000000000, 0.000000000000000000, 1.000000000000000000 ) ) ;
#11642 = CARTESIAN_POINT ( 'NONE',  ( 10.00000000000000178, 0.000000000000000000, 0.000000000000000000 ) ) ;
#11643 = ORIENTED_EDGE ( 'NONE', *, *, #803, .F. ) ;
#11644 = DIRECTION ( 'NONE',  ( 0.000000000000000000, 0.000000000000000000, 1.000000000000000000 ) ) ;
#11645 = ORIENTED_EDGE ( 'NONE', *, *, #3376, .T. ) ;
#11646 = PRODUCT_DEFINITION_SHAPE ( 'NONE', 'NONE',  #18816 ) ;
#11647 = DIRECTION ( 'NONE',  ( -0.000000000000000000, -0.000000000000000000, 1.000000000000000000 ) ) ;
#11648 = DIRECTION ( 'NONE',  ( 0.000000000000000000, 0.000000000000000000, 1.000000000000000000 ) ) ;
#11649 = VERTEX_POINT ( 'NONE', #10370 ) ;
#11650 = SHAPE_DEFINITION_REPRESENTATION ( #5561, #2386 ) ;
#11651 = CIRCLE ( 'NONE', #16511, 2.649999999999992806 ) ;
#11652 = VERTEX_POINT ( 'NONE', #3049 ) ;
#11653 = CIRCLE ( 'NONE', #691, 63.00000000006298961 ) ;
#11654 = CIRCLE ( 'NONE', #9828, 12.00000000001200462 ) ;
#11655 = DIRECTION ( 'NONE',  ( 0.000000000000000000, 0.000000000000000000, 1.000000000000000000 ) ) ;
#11656 = CARTESIAN_POINT ( 'NONE',  ( 10.00000000000000000, 53.92768374110892893, -16.45250512421876010 ) ) ;
#11657 = CARTESIAN_POINT ( 'NONE',  ( 10.00000000000000178, 0.000000000000000000, 0.000000000000000000 ) ) ;
#11658 = CARTESIAN_POINT ( 'NONE',  ( 10.00000000000000000, 0.000000000000000000, 0.000000000000000000 ) ) ;
#11659 = VECTOR ( 'NONE', #17199, 1000.000000000000000 ) ;
#11660 = DIRECTION ( 'NONE',  ( -1.000000000000000000, 0.000000000000000000, 0.000000000000000000 ) ) ;
#11661 = CIRCLE ( 'NONE', #2845, 2.649999999999999467 ) ;
#11662 = DIRECTION ( 'NONE',  ( -0.000000000000000000, -0.000000000000000000, -1.000000000000000000 ) ) ;
#11663 = VERTEX_POINT ( 'NONE', #8930 ) ;
#11664 = EDGE_CURVE ( 'NONE', #11128, #3467, #6296, .T. ) ;
#11665 = EDGE_CURVE ( 'NONE', #14997, #923, #9334, .T. ) ;
#11666 = CARTESIAN_POINT ( 'NONE',  ( -36.40576474687247099, 0.000000000000000000, 26.45033635316149301 ) ) ;
#11667 = DIRECTION ( 'NONE',  ( -1.000000000000000000, 0.000000000000000000, 0.000000000000000000 ) ) ;
#11668 = DIRECTION ( 'NONE',  ( -0.000000000000000000, -0.000000000000000000, -1.000000000000000000 ) ) ;
#11669 = ORIENTED_EDGE ( 'NONE', *, *, #976, .F. ) ;
#11670 = ORIENTED_EDGE ( 'NONE', *, *, #5058, .T. ) ;
#11671 = CYLINDRICAL_SURFACE ( 'NONE', #15985, 24.00000000002399858 ) ;
#11672 = DIRECTION ( 'NONE',  ( 0.000000000000000000, 0.000000000000000000, 1.000000000000000000 ) ) ;
#11673 = PRODUCT_RELATED_PRODUCT_CATEGORY ( 'part', '', ( #15750 ) ) ;
#11674 = ORIENTED_EDGE ( 'NONE', *, *, #13242, .F. ) ;
#11675 = ADVANCED_FACE ( 'NONE', ( #8656 ), #7229, .F. ) ;
#11676 = CIRCLE ( 'NONE', #412, 24.00000000002399858 ) ;
#11677 = DIRECTION ( 'NONE',  ( 1.000000000000000000, 0.000000000000000000, 0.000000000000000000 ) ) ;
#11678 = DIRECTION ( 'NONE',  ( 0.000000000000000000, 0.000000000000000000, -1.000000000000000000 ) ) ;
#11679 = EDGE_CURVE ( 'NONE', #5010, #9182, #17556, .T. ) ;
#11680 = DIRECTION ( 'NONE',  ( -1.000000000000000000, 0.000000000000000000, -0.000000000000000000 ) ) ;
#11681 = ORIENTED_EDGE ( 'NONE', *, *, #3067, .T. ) ;
#11682 = DIRECTION ( 'NONE',  ( -1.000000000000000000, 0.000000000000000000, 0.000000000000000000 ) ) ;
#11683 = ORIENTED_EDGE ( 'NONE', *, *, #6384, .T. ) ;
#11684 = UNCERTAINTY_MEASURE_WITH_UNIT (LENGTH_MEASURE( 1.000000000000000082E-05 ), #18254, 'distance_accuracy_value', 'NONE');
#11685 = DIRECTION ( 'NONE',  ( 0.000000000000000000, 0.000000000000000000, 1.000000000000000000 ) ) ;
#11686 = VERTEX_POINT ( 'NONE', #4469 ) ;
#11688 = ORIENTED_EDGE ( 'NONE', *, *, #10520, .F. ) ;
#11687 = EDGE_CURVE ( 'NONE', #3393, #8632, #15128, .T. ) ;
#11689 = ADVANCED_FACE ( 'NONE', ( #14657 ), #5985, .F. ) ;
#11690 = CARTESIAN_POINT ( 'NONE',  ( -90.00000000009001155, -13.00000000000001776, -1.691355389077386325E-15 ) ) ;
#11691 = CARTESIAN_POINT ( 'NONE',  ( -90.00000000009001155, -38.00000000000000000, -40.00000000000000000 ) ) ;
#11692 = VERTEX_POINT ( 'NONE', #6548 ) ;
#11693 = ORIENTED_EDGE ( 'NONE', *, *, #13681, .F. ) ;
#11694 = DIRECTION ( 'NONE',  ( 0.000000000000000000, 0.000000000000000000, 1.000000000000000000 ) ) ;
#11695 = EDGE_CURVE ( 'NONE', #14348, #12626, #15229, .T. ) ;
#11696 = ORIENTED_EDGE ( 'NONE', *, *, #12039, .F. ) ;
#11697 = PLANE ( 'NONE',  #12450 ) ;
#11698 = ADVANCED_FACE ( 'NONE', ( #7979 ), #3614, .T. ) ;
#11699 =( REPRESENTATION_RELATIONSHIP ('NONE','NONE', #11014, #16765 ) REPRESENTATION_RELATIONSHIP_WITH_TRANSFORMATION ( #10861 )SHAPE_REPRESENTATION_RELATIONSHIP( ) );
#11700 = ADVANCED_FACE ( 'NONE', ( #561 ), #13425, .T. ) ;
#11701 =( GEOMETRIC_REPRESENTATION_CONTEXT ( 3 ) GLOBAL_UNCERTAINTY_ASSIGNED_CONTEXT ( ( #5381 ) ) GLOBAL_UNIT_ASSIGNED_CONTEXT ( ( #13730, #18466, #10761 ) ) REPRESENTATION_CONTEXT ( 'NONE', 'WORKASPACE' ) );
#11702 = CARTESIAN_POINT ( 'NONE',  ( -56.50000000009000445, -30.00000000000000000, 2.650000000000367173 ) ) ;
#11703 = ORIENTED_EDGE ( 'NONE', *, *, #14864, .T. ) ;
#11704 = VERTEX_POINT ( 'NONE', #7890 ) ;
#11705 = FACE_OUTER_BOUND ( 'NONE', #15514, .T. ) ;
#11706 = CARTESIAN_POINT ( 'NONE',  ( 0.000000000000000000, 10.00000000000000000, 0.000000000000000000 ) ) ;
#11707 = LINE ( 'NONE', #17610, #18470 ) ;
#11708 = ORIENTED_EDGE ( 'NONE', *, *, #15415, .F. ) ;
#11709 = DIRECTION ( 'NONE',  ( -1.000000000000000000, 0.000000000000000000, 0.000000000000000000 ) ) ;
#11710 = DIRECTION ( 'NONE',  ( 0.000000000000000000, 0.000000000000000000, 1.000000000000000000 ) ) ;
#11711 = CARTESIAN_POINT ( 'NONE',  ( -26.29305231718584324, -30.00000000000000000, 19.10302069950530779 ) ) ;
#11712 = CARTESIAN_POINT ( 'NONE',  ( 0.000000000000000000, -1.178949249685214307, 2.042000000000001592 ) ) ;
#11713 = EDGE_LOOP ( 'NONE', ( #13988, #2647 ) ) ;
#11714 = CYLINDRICAL_SURFACE ( 'NONE', #7586, 12.00000000001200462 ) ;
#11715 = DIRECTION ( 'NONE',  ( 0.000000000000000000, 0.000000000000000000, 1.000000000000000000 ) ) ;
#11716 = ORIENTED_EDGE ( 'NONE', *, *, #14450, .F. ) ;
#11717 = LINE ( 'NONE', #8851, #16392 ) ;
#11718 = DIRECTION ( 'NONE',  ( -0.000000000000000000, 0.000000000000000000, 1.000000000000000000 ) ) ;
#11719 = VECTOR ( 'NONE', #15125, 1000.000000000000000 ) ;
#11720 = CIRCLE ( 'NONE', #17505, 20.00000000000000000 ) ;
#11721 = EDGE_CURVE ( 'NONE', #16237, #3613, #13513, .T. ) ;
#11722 = ORIENTED_EDGE ( 'NONE', *, *, #5586, .T. ) ;
#11723 = EDGE_CURVE ( 'NONE', #8620, #15269, #8413, .T. ) ;
#11724 = CARTESIAN_POINT ( 'NONE',  ( 10.00000000000000000, -53.29895248911662264, -18.38754094778296277 ) ) ;
#11725 = CARTESIAN_POINT ( 'NONE',  ( 10.00000000000000000, 27.94286728106393269, 15.73043801031642808 ) ) ;
#11726 = AXIS2_PLACEMENT_3D ( 'NONE', #8144, #18239, #6898 ) ;
#11727 = ORIENTED_EDGE ( 'NONE', *, *, #9117, .T. ) ;
#11728 = CIRCLE ( 'NONE', #7773, 2.055000000000000160 ) ;
#11729 = CARTESIAN_POINT ( 'NONE',  ( -10.00000000000000000, 0.000000000000000000, 0.000000000000000000 ) ) ;
#11730 = LINE ( 'NONE', #17637, #2683 ) ;
#11731 = FACE_OUTER_BOUND ( 'NONE', #17396, .T. ) ;
#11732 = FACE_OUTER_BOUND ( 'NONE', #2809, .T. ) ;
#11733 = ORIENTED_EDGE ( 'NONE', *, *, #7387, .F. ) ;
#11734 = CARTESIAN_POINT ( 'NONE',  ( 5.000000000000000000, -15.68049343255974826, -29.03656532225581088 ) ) ;
#11735 = ORIENTED_EDGE ( 'NONE', *, *, #4927, .T. ) ;
#11736 = CARTESIAN_POINT ( 'NONE',  ( 0.000000000000000000, -32.70783759231089505, 4.381479206522877590 ) ) ;
#11737 = CARTESIAN_POINT ( 'NONE',  ( -26.29305231718568336, -34.99999999999999289, -16.45302069950552237 ) ) ;
#11738 = ORIENTED_EDGE ( 'NONE', *, *, #10639, .T. ) ;
#11739 = AXIS2_PLACEMENT_3D ( 'NONE', #4426, #4340, #15868 ) ;
#11740 = CIRCLE ( 'NONE', #6264, 27.50000000000000000 ) ;
#11741 = EDGE_CURVE ( 'NONE', #17771, #17376, #8120, .T. ) ;
#11742 = APPLICATION_PROTOCOL_DEFINITION ( 'draft international standard', 'automotive_design', 1998, #8877 ) ;
#11743 = ORIENTED_EDGE ( 'NONE', *, *, #4591, .T. ) ;
#11744 = AXIS2_PLACEMENT_3D ( 'NONE', #1197, #2997, #10044 ) ;
#11745 = VECTOR ( 'NONE', #9239, 1000.000000000000000 ) ;
#11746 = DIRECTION ( 'NONE',  ( 0.000000000000000000, -1.000000000000000000, -1.040834085585042960E-14 ) ) ;
#11747 = CARTESIAN_POINT ( 'NONE',  ( 4.211140560182196957, 2.431303136016536470, -3.745885042887433514 ) ) ;
#11748 = CIRCLE ( 'NONE', #3543, 25.00000000000000000 ) ;
#11749 = CARTESIAN_POINT ( 'NONE',  ( 10.00000000000000000, -4.007856633823827508, 62.87238730325619684 ) ) ;
#11750 = EDGE_CURVE ( 'NONE', #13167, #16305, #5015, .T. ) ;
#11751 = DIRECTION ( 'NONE',  ( 0.000000000000000000, 0.000000000000000000, 1.000000000000000000 ) ) ;
#11752 = AXIS2_PLACEMENT_3D ( 'NONE', #601, #6698, #10966 ) ;
#11753 = DIRECTION ( 'NONE',  ( -1.000000000000000000, -0.000000000000000000, -0.000000000000000000 ) ) ;
#11754 = DIRECTION ( 'NONE',  ( 0.000000000000000000, -0.3090169943749351278, -0.9510565162951575280 ) ) ;
#11755 = CIRCLE ( 'NONE', #5682, 2.649999999999999467 ) ;
#11756 = DIRECTION ( 'NONE',  ( 0.000000000000000000, 0.000000000000000000, 1.000000000000000000 ) ) ;
#11757 = ORIENTED_EDGE ( 'NONE', *, *, #2740, .T. ) ;
#11758 = ADVANCED_FACE ( 'NONE', ( #9129 ), #2086, .T. ) ;
#11759 = DIRECTION ( 'NONE',  ( 0.000000000000000000, 0.000000000000000000, 1.000000000000000000 ) ) ;
#11760 = LINE ( 'NONE', #17386, #16525 ) ;
#11761 = DIRECTION ( 'NONE',  ( -1.000000000000000000, -0.000000000000000000, -0.000000000000000000 ) ) ;
#11762 = ORIENTED_EDGE ( 'NONE', *, *, #14370, .T. ) ;
#11763 = EDGE_LOOP ( 'NONE', ( #17929, #12945, #6553, #834 ) ) ;
#11764 = CARTESIAN_POINT ( 'NONE',  ( 0.000000000000000000, 62.87238730325621106, 4.007856633823609016 ) ) ;
#11765 = PLANE ( 'NONE',  #995 ) ;
#11766 = ORIENTED_EDGE ( 'NONE', *, *, #1665, .F. ) ;
#11767 = AXIS2_PLACEMENT_3D ( 'NONE', #17980, #3330, #4646 ) ;
#11768 = AXIS2_PLACEMENT_3D ( 'NONE', #3034, #2655, #11694 ) ;
#11769 = AXIS2_PLACEMENT_3D ( 'NONE', #3352, #10668, #10574 ) ;
#11770 = CIRCLE ( 'NONE', #11477, 2.041999999999999815 ) ;
#11771 = AXIS2_PLACEMENT_3D ( 'NONE', #7228, #11619, #10094 ) ;
#11772 = DIRECTION ( 'NONE',  ( 0.000000000000000000, 0.9510565162951521989, 0.3090169943749515036 ) ) ;
#11773 = CARTESIAN_POINT ( 'NONE',  ( -0.1404048886732797152, -4.699864953788083888, -3.686887068327043160 ) ) ;
#11774 = DIRECTION ( 'NONE',  ( -1.000000000000000000, 0.000000000000000000, -0.000000000000000000 ) ) ;
#11775 = ORIENTED_EDGE ( 'NONE', *, *, #11525, .F. ) ;
#11776 = CARTESIAN_POINT ( 'NONE',  ( 2.682243648011666703, 3.070208061305304881, -0.04852650426601266831 ) ) ;
#11777 = AXIS2_PLACEMENT_3D ( 'NONE', #17425, #4376, #10179 ) ;
#11778 = ORIENTED_EDGE ( 'NONE', *, *, #18088, .T. ) ;
#11779 = FACE_OUTER_BOUND ( 'NONE', #8741, .T. ) ;
#11780 = ORIENTED_EDGE ( 'NONE', *, *, #8215, .F. ) ;
#11781 = VERTEX_POINT ( 'NONE', #14849 ) ;
#11782 = VECTOR ( 'NONE', #458, 1000.000000000000000 ) ;
#11783 = DIRECTION ( 'NONE',  ( 1.000000000000000000, -3.469446951953611231E-16, 0.000000000000000000 ) ) ;
#11784 = CARTESIAN_POINT ( 'NONE',  ( 0.000000000000000000, 10.00000000000000000, 0.000000000000000000 ) ) ;
#11785 = ORIENTED_EDGE ( 'NONE', *, *, #1205, .T. ) ;
#11786 = VERTEX_POINT ( 'NONE', #9029 ) ;
#11787 = CIRCLE ( 'NONE', #5998, 5.000000000000000000 ) ;
#11788 = DIRECTION ( 'NONE',  ( 0.000000000000000000, 0.000000000000000000, -1.000000000000000000 ) ) ;
#11789 = ORIENTED_EDGE ( 'NONE', *, *, #18297, .T. ) ;
#11790 = DIRECTION ( 'NONE',  ( 0.000000000000000000, -0.5877852522924624790, -0.8090169943749551118 ) ) ;
#11791 = AXIS2_PLACEMENT_3D ( 'NONE', #18640, #2830, #16070 ) ;
#11792 = EDGE_CURVE ( 'NONE', #10824, #11956, #6018, .T. ) ;
#11793 = EDGE_CURVE ( 'NONE', #7149, #18521, #1885, .T. ) ;
#11794 = AXIS2_PLACEMENT_3D ( 'NONE', #1848, #7650, #13477 ) ;
#11795 = DIRECTION ( 'NONE',  ( 0.000000000000000000, 0.000000000000000000, -1.000000000000000000 ) ) ;
#11796 = EDGE_CURVE ( 'NONE', #833, #17767, #7687, .T. ) ;
#11797 = CIRCLE ( 'NONE', #18806, 5.000000000000000000 ) ;
#11798 = ORIENTED_EDGE ( 'NONE', *, *, #7499, .T. ) ;
#11799 = EDGE_CURVE ( 'NONE', #14286, #9048, #3508, .T. ) ;
#11800 = EDGE_LOOP ( 'NONE', ( #1429, #15194, #9554, #2167 ) ) ;
#11801 = CARTESIAN_POINT ( 'NONE',  ( 0.000000000000000000, 0.000000000000000000, 0.000000000000000000 ) ) ;
#11802 = LINE ( 'NONE', #1605, #15347 ) ;
#11803 = CARTESIAN_POINT ( 'NONE',  ( 0.000000000000000000, 0.000000000000000000, 0.000000000000000000 ) ) ;
#11804 = ORIENTED_EDGE ( 'NONE', *, *, #7484, .F. ) ;
#11805 = CARTESIAN_POINT ( 'NONE',  ( -4.000000000000000000, -1.680117682357936904, -3.316611593218794951 ) ) ;
#11806 = DIRECTION ( 'NONE',  ( 0.000000000000000000, 0.000000000000000000, 1.000000000000000000 ) ) ;
#11807 = CARTESIAN_POINT ( 'NONE',  ( 10.00000000000000000, 22.07705612348840063, 14.19907017806876404 ) ) ;
#11808 = CIRCLE ( 'NONE', #6020, 24.00000000002399858 ) ;
#11809 = FACE_BOUND ( 'NONE', #2339, .T. ) ;
#11810 = VERTEX_POINT ( 'NONE', #12180 ) ;
#11811 = DIRECTION ( 'NONE',  ( -0.7071067811865364705, 0.000000000000000000, 0.7071067811865584529 ) ) ;
#11812 = CARTESIAN_POINT ( 'NONE',  ( 10.00000000000000000, 0.000000000000000000, 0.000000000000000000 ) ) ;
#11813 = AXIS2_PLACEMENT_3D ( 'NONE', #18008, #12200, #6770 ) ;
#11814 = VERTEX_POINT ( 'NONE', #4847 ) ;
#11815 = DIRECTION ( 'NONE',  ( 0.000000000000000000, 0.000000000000000000, -1.000000000000000000 ) ) ;
#11816 = CARTESIAN_POINT ( 'NONE',  ( 10.00000000000000000, 0.000000000000000000, 0.000000000000000000 ) ) ;
#11817 =( GEOMETRIC_REPRESENTATION_CONTEXT ( 3 ) GLOBAL_UNCERTAINTY_ASSIGNED_CONTEXT ( ( #12240 ) ) GLOBAL_UNIT_ASSIGNED_CONTEXT ( ( #2210, #13824, #18216 ) ) REPRESENTATION_CONTEXT ( 'NONE', 'WORKASPACE' ) );
#11818 = AXIS2_PLACEMENT_3D ( 'NONE', #5145, #7999, #15249 ) ;
#11819 = EDGE_CURVE ( 'NONE', #16951, #8859, #6617, .T. ) ;
#11820 = ORIENTED_EDGE ( 'NONE', *, *, #4263, .F. ) ;
#11821 = DIRECTION ( 'NONE',  ( -0.000000000000000000, -0.000000000000000000, -1.000000000000000000 ) ) ;
#11822 = CARTESIAN_POINT ( 'NONE',  ( 0.000000000000000000, -62.72529079327802748, -5.876895005583096854 ) ) ;
#11823 = AXIS2_PLACEMENT_3D ( 'NONE', #5231, #9427, #12570 ) ;
#11824 = ORIENTED_EDGE ( 'NONE', *, *, #17289, .T. ) ;
#11825 = AXIS2_PLACEMENT_3D ( 'NONE', #11401, #11510, #6940 ) ;
#11826 = CARTESIAN_POINT ( 'NONE',  ( 10.00000000000000000, -10.11537145609335830, -55.33199130079796646 ) ) ;
#11827 = EDGE_CURVE ( 'NONE', #13797, #2843, #16466, .T. ) ;
#11828 = DIRECTION ( 'NONE',  ( 1.000000000000000000, 0.000000000000000000, 0.000000000000000000 ) ) ;
#11829 = LINE ( 'NONE', #2878, #3890 ) ;
#11830 = CYLINDRICAL_SURFACE ( 'NONE', #17996, 5.000000000000004441 ) ;
#11831 = CARTESIAN_POINT ( 'NONE',  ( 10.00000000000000000, 20.41355805489615705, 19.44239304137382973 ) ) ;
#11832 = ORIENTED_EDGE ( 'NONE', *, *, #497, .F. ) ;
#11833 = CYLINDRICAL_SURFACE ( 'NONE', #17606, 0.7500000000000000000 ) ;
#11834 = ORIENTED_EDGE ( 'NONE', *, *, #11349, .T. ) ;
#11835 = CARTESIAN_POINT ( 'NONE',  ( -1.999999999999999556, 3.464101615137754830, -3.142992957459232795 ) ) ;
#11836 = CIRCLE ( 'NONE', #14579, 12.00000000001200640 ) ;
#11837 = ORIENTED_EDGE ( 'NONE', *, *, #8496, .F. ) ;
#11838 = ORIENTED_EDGE ( 'NONE', *, *, #10018, .T. ) ;
#11839 = ORIENTED_EDGE ( 'NONE', *, *, #1219, .T. ) ;
#11840 = CARTESIAN_POINT ( 'NONE',  ( -82.50000000008999734, -10.00000000000001954, -5.777138986694819161E-16 ) ) ;
#11841 = CARTESIAN_POINT ( 'NONE',  ( 4.101954839143203912, 2.368264730583012234, -3.681130640444374436 ) ) ;
#11842 = AXIS2_PLACEMENT_3D ( 'NONE', #15726, #1430, #2677 ) ;
#11843 = DIRECTION ( 'NONE',  ( -1.000000000000000000, -0.000000000000000000, -0.000000000000000000 ) ) ;
#11844 = EDGE_CURVE ( 'NONE', #16169, #14282, #18164, .T. ) ;
#11845 = CARTESIAN_POINT ( 'NONE',  ( 10.00000000000000000, -48.50907078259351835, -40.19788616105662982 ) ) ;
#11846 = CARTESIAN_POINT ( 'NONE',  ( 5.560781378645573980, 6.809993116116507654E-16, -4.000000000000000000 ) ) ;
#11847 = FACE_OUTER_BOUND ( 'NONE', #13567, .T. ) ;
#11848 = CARTESIAN_POINT ( 'NONE',  ( 3.309651814758564736, -5.455921364805393026, -1.000000000000000000 ) ) ;
#11849 = LINE ( 'NONE', #10604, #8789 ) ;
#11850 = ORIENTED_EDGE ( 'NONE', *, *, #4240, .F. ) ;
#11851 = CYLINDRICAL_SURFACE ( 'NONE', #1695, 24.00000000002399858 ) ;
#11852 = CARTESIAN_POINT ( 'NONE',  ( 0.000000000000000000, 0.000000000000000000, -1.000000000000000000 ) ) ;
#11853 = LINE ( 'NONE', #16235, #2679 ) ;
#11854 = ORIENTED_EDGE ( 'NONE', *, *, #18337, .F. ) ;
#11855 = ORIENTED_EDGE ( 'NONE', *, *, #10515, .F. ) ;
#11856 = LINE ( 'NONE', #147, #8407 ) ;
#11857 = FACE_OUTER_BOUND ( 'NONE', #36, .T. ) ;
#11858 = VERTEX_POINT ( 'NONE', #658 ) ;
#11859 = VECTOR ( 'NONE', #15203, 1000.000000000000114 ) ;
#11860 = EDGE_CURVE ( 'NONE', #8916, #3012, #16645, .T. ) ;
#11861 = EDGE_CURVE ( 'NONE', #6419, #3486, #15412, .T. ) ;
#11862 = DIRECTION ( 'NONE',  ( 0.000000000000000000, 0.000000000000000000, 1.000000000000000000 ) ) ;
#11863 = FACE_OUTER_BOUND ( 'NONE', #4650, .T. ) ;
#11864 = CARTESIAN_POINT ( 'NONE',  ( 10.00000000000000000, 0.000000000000000000, 0.000000000000000000 ) ) ;
#11865 = ORIENTED_EDGE ( 'NONE', *, *, #11750, .T. ) ;
#11866 = CARTESIAN_POINT ( 'NONE',  ( 0.3208286057739604957, -4.433571671609698228, -0.3503314178412692548 ) ) ;
#11867 = EDGE_LOOP ( 'NONE', ( #2815, #10943, #7561, #1889, #5963, #14559, #9970 ) ) ;
#11868 = CIRCLE ( 'NONE', #12789, 26.24900000002625688 ) ;
#11869 = FACE_OUTER_BOUND ( 'NONE', #8152, .T. ) ;
#11870 = ORIENTED_EDGE ( 'NONE', *, *, #16685, .T. ) ;
#11871 = AXIS2_PLACEMENT_3D ( 'NONE', #11260, #1539, #17632 ) ;
#11872 = DIRECTION ( 'NONE',  ( 0.000000000000000000, 0.000000000000000000, -1.000000000000000000 ) ) ;
#11873 = DIRECTION ( 'NONE',  ( -0.000000000000000000, -1.000000000000000000, -0.000000000000000000 ) ) ;
#11874 = ORIENTED_EDGE ( 'NONE', *, *, #1066, .T. ) ;
#11875 = ORIENTED_EDGE ( 'NONE', *, *, #16775, .F. ) ;
#11876 = DIRECTION ( 'NONE',  ( -1.000000000000000000, 0.000000000000000000, -0.000000000000000000 ) ) ;
#11877 = VERTEX_POINT ( 'NONE', #3894 ) ;
#11878 = CARTESIAN_POINT ( 'NONE',  ( 0.000000000000000000, 0.000000000000000000, 0.000000000000000000 ) ) ;
#11879 = CIRCLE ( 'NONE', #3684, 2.649999999999999467 ) ;
#11880 = CARTESIAN_POINT ( 'NONE',  ( 2.500000000000000000, 2.253471898105738645E-15, 2.041999999999999815 ) ) ;
#11881 = EDGE_LOOP ( 'NONE', ( #8817, #2775, #16581, #14977 ) ) ;
#11882 = ORIENTED_EDGE ( 'NONE', *, *, #112, .T. ) ;
#11883 = DIRECTION ( 'NONE',  ( 0.000000000000000000, 0.000000000000000000, 1.000000000000000000 ) ) ;
#11884 = LINE ( 'NONE', #14741, #3194 ) ;
#11885 = CARTESIAN_POINT ( 'NONE',  ( 10.00000000000000000, 0.000000000000000000, 0.000000000000000000 ) ) ;
#11886 = EDGE_LOOP ( 'NONE', ( #6816, #5820, #6332, #12756 ) ) ;
#11887 = DIRECTION ( 'NONE',  ( -1.000000000000000000, 0.000000000000000000, -0.000000000000000000 ) ) ;
#11888 = FACE_OUTER_BOUND ( 'NONE', #8369, .T. ) ;
#11889 = DIRECTION ( 'NONE',  ( -1.000000000000000000, -0.000000000000000000, -0.000000000000000000 ) ) ;
#11890 = CARTESIAN_POINT ( 'NONE',  ( -2.688821387764050996E-14, -4.618802153517012954, -0.4999999999999995559 ) ) ;
#11891 = ORIENTED_EDGE ( 'NONE', *, *, #12267, .F. ) ;
#11892 = FACE_OUTER_BOUND ( 'NONE', #3840, .T. ) ;
#11893 = EDGE_CURVE ( 'NONE', #16334, #17597, #9591, .T. ) ;
#11894 = AXIS2_PLACEMENT_3D ( 'NONE', #16247, #3203, #15375 ) ;
#11895 = FILL_AREA_STYLE_COLOUR ( '', #13270 ) ;
#11896 = EDGE_CURVE ( 'NONE', #9267, #1277, #7206, .T. ) ;
#11897 = ORIENTED_EDGE ( 'NONE', *, *, #18440, .T. ) ;
#11898 = DIRECTION ( 'NONE',  ( 0.000000000000000000, -0.9510565162951565288, 0.3090169943749382364 ) ) ;
#11899 = FACE_OUTER_BOUND ( 'NONE', #2101, .T. ) ;
#11900 = EDGE_CURVE ( 'NONE', #15277, #8733, #17856, .T. ) ;
#11901 = ADVANCED_FACE ( 'NONE', ( #16752 ), #2341, .F. ) ;
#11902 = EDGE_LOOP ( 'NONE', ( #15327, #10580, #3263, #7633 ) ) ;
#11903 = CARTESIAN_POINT ( 'NONE',  ( -79.64793068852927149, -34.99999999999999289, 34.51039329588763849 ) ) ;
#11904 = DIRECTION ( 'NONE',  ( -1.000000000000000000, 0.000000000000000000, 0.000000000000000000 ) ) ;
#11905 = EDGE_CURVE ( 'NONE', #13289, #13886, #3268, .T. ) ;
#11906 = EDGE_LOOP ( 'NONE', ( #16186, #12444, #13980, #1799 ) ) ;
#11907 = DIRECTION ( 'NONE',  ( -1.000000000000000000, 0.000000000000000000, -0.000000000000000000 ) ) ;
#11908 = DIRECTION ( 'NONE',  ( 0.000000000000000000, 0.000000000000000000, 1.000000000000000000 ) ) ;
#11909 = VECTOR ( 'NONE', #11611, 1000.000000000000000 ) ;
#11910 = CIRCLE ( 'NONE', #10087, 26.24900000002625333 ) ;
#11911 = CARTESIAN_POINT ( 'NONE',  ( 10.00000000000000000, -40.58063702438316511, -39.14194549634407139 ) ) ;
#11912 = FACE_OUTER_BOUND ( 'NONE', #7373, .T. ) ;
#11913 = DIRECTION ( 'NONE',  ( 0.000000000000000000, 0.000000000000000000, 1.000000000000000000 ) ) ;
#11914 = ORIENTED_EDGE ( 'NONE', *, *, #10154, .T. ) ;
#11915 = FACE_OUTER_BOUND ( 'NONE', #17497, .T. ) ;
#11916 = ORIENTED_EDGE ( 'NONE', *, *, #18550, .F. ) ;
#11917 = EDGE_CURVE ( 'NONE', #2800, #16028, #2546, .T. ) ;
#11918 = ADVANCED_FACE ( 'NONE', ( #12749 ), #15601, .F. ) ;
#11919 =( NAMED_UNIT ( * ) SI_UNIT ( $, .STERADIAN. ) SOLID_ANGLE_UNIT ( ) );
#11920 = CARTESIAN_POINT ( 'NONE',  ( 10.00000000000000000, 0.000000000000000000, 0.000000000000000000 ) ) ;
#11921 = VERTEX_POINT ( 'NONE', #12551 ) ;
#11922 = ITEM_DEFINED_TRANSFORMATION ( 'NONE', 'NONE', #7744,  #8017 ) ;
#11923 = EDGE_CURVE ( 'NONE', #13117, #1965, #15428, .T. ) ;
#11924 = ORIENTED_EDGE ( 'NONE', *, *, #15871, .F. ) ;
#11925 = ADVANCED_FACE ( 'NONE', ( #6744 ), #5511, .F. ) ;
#11926 = CIRCLE ( 'NONE', #15274, 4.799999999999998934 ) ;
#11927 = ORIENTED_EDGE ( 'NONE', *, *, #9683, .F. ) ;
#11928 = VERTEX_POINT ( 'NONE', #12843 ) ;
#11929 = LINE ( 'NONE', #8964, #18139 ) ;
#11930 = DIRECTION ( 'NONE',  ( 0.000000000000000000, 0.000000000000000000, 1.000000000000000000 ) ) ;
#11931 = FACE_OUTER_BOUND ( 'NONE', #18280, .T. ) ;
#11932 = DIRECTION ( 'NONE',  ( -1.000000000000000000, -0.000000000000000000, -0.000000000000000000 ) ) ;
#11933 = DIRECTION ( 'NONE',  ( -1.000000000000000000, 0.000000000000000000, 0.000000000000000000 ) ) ;
#11934 = CARTESIAN_POINT ( 'NONE',  ( 0.000000000000000000, -1.178949249685213863, 2.042000000000001148 ) ) ;
#11935 = CARTESIAN_POINT ( 'NONE',  ( -90.70833251482494575, 1.000000000000014655, -4.949572208642815774 ) ) ;
#11936 = DIRECTION ( 'NONE',  ( 1.000000000000000000, 0.000000000000000000, 0.000000000000000000 ) ) ;
#11937 = ORIENTED_EDGE ( 'NONE', *, *, #10280, .T. ) ;
#11938 = CIRCLE ( 'NONE', #15590, 2.649999999999992806 ) ;
#11939 = CARTESIAN_POINT ( 'NONE',  ( 1.411581201560190495E-15, 4.862606272033091592, -3.745885042887436622 ) ) ;
#11940 = CIRCLE ( 'NONE', #4948, 20.00000000000000000 ) ;
#11941 = DIRECTION ( 'NONE',  ( 0.000000000000000000, -0.5877852522924801315, 0.8090169943749422332 ) ) ;
#11942 = VERTEX_POINT ( 'NONE', #11114 ) ;
#11943 = ORIENTED_EDGE ( 'NONE', *, *, #641, .T. ) ;
#11944 = CLOSED_SHELL ( 'NONE', ( #18783, #3886, #11901, #16124, #3308, #7828, #14825, #4660, #8878, #2239, #13556, #14932, #4533, #13769, #988, #1096, #13262, #8197, #5421, #16954, #10496, #5524, #9172, #6832, #13307, #11582, #15984, #18073, #1263, #3195, #15711, #6564 ) ) ;
#11945 =( REPRESENTATION_RELATIONSHIP ('NONE','NONE', #11014, #2517 ) REPRESENTATION_RELATIONSHIP_WITH_TRANSFORMATION ( #5243 )SHAPE_REPRESENTATION_RELATIONSHIP( ) );
#11946 = CARTESIAN_POINT ( 'NONE',  ( -2.171643655288372443, 3.365003104552320767, 2.541098841762897165E-18 ) ) ;
#11947 = CARTESIAN_POINT ( 'NONE',  ( -79.64793068852898728, -25.00000000000000000, -31.86039329588756530 ) ) ;
#11948 = CARTESIAN_POINT ( 'NONE',  ( 5.000000000000000000, -62.87238730325618263, -4.007856633824053105 ) ) ;
#11949 = ORIENTED_EDGE ( 'NONE', *, *, #7905, .T. ) ;
#11950 = EDGE_CURVE ( 'NONE', #10165, #906, #5394, .T. ) ;
#11951 = AXIS2_PLACEMENT_3D ( 'NONE', #830, #2335, #2241 ) ;
#11952 = FACE_OUTER_BOUND ( 'NONE', #15381, .T. ) ;
#11953 = FACE_OUTER_BOUND ( 'NONE', #8529, .T. ) ;
#11954 = AXIS2_PLACEMENT_3D ( 'NONE', #6183, #7617, #470 ) ;
#11955 = CARTESIAN_POINT ( 'NONE',  ( 10.00000000000000000, 16.45250512421934630, -53.92768374110874419 ) ) ;
#11956 = VERTEX_POINT ( 'NONE', #5214 ) ;
#11957 = FACE_OUTER_BOUND ( 'NONE', #17045, .T. ) ;
#11958 = ORIENTED_EDGE ( 'NONE', *, *, #507, .F. ) ;
#11959 = DIRECTION ( 'NONE',  ( 2.031314180040284764E-16, 1.000000000000000000, 1.301042606982601623E-16 ) ) ;
#11960 = ORIENTED_EDGE ( 'NONE', *, *, #986, .T. ) ;
#11961 = CYLINDRICAL_SURFACE ( 'NONE', #17823, 24.00000000002399858 ) ;
#11962 = CARTESIAN_POINT ( 'NONE',  ( -1.257172072275743346, 3.892973519171203378, -3.433252694550776862 ) ) ;
#11963 = VERTEX_POINT ( 'NONE', #8274 ) ;
#11964 = ORIENTED_EDGE ( 'NONE', *, *, #17754, .F. ) ;
#11965 = DIRECTION ( 'NONE',  ( -1.000000000000000000, 0.000000000000000000, 0.000000000000000000 ) ) ;
#11966 = ADVANCED_FACE ( 'NONE', ( #8461, #6831 ), #18642, .T. ) ;
#11967 = ORIENTED_EDGE ( 'NONE', *, *, #13664, .F. ) ;
#11968 = DIRECTION ( 'NONE',  ( -1.000000000000000000, -0.000000000000000000, 0.000000000000000000 ) ) ;
#11969 = CARTESIAN_POINT ( 'NONE',  ( 10.00000000000000000, 0.000000000000000000, 0.000000000000000000 ) ) ;
#11970 = EDGE_LOOP ( 'NONE', ( #11418, #13128 ) ) ;
#11971 = VERTEX_POINT ( 'NONE', #2645 ) ;
#11972 = CARTESIAN_POINT ( 'NONE',  ( 5.000000000000000000, -29.75305054077462330, -14.27431201565557117 ) ) ;
#11973 = DIRECTION ( 'NONE',  ( -1.000000000000000000, -0.000000000000000000, -0.000000000000000000 ) ) ;
#11974 = DIRECTION ( 'NONE',  ( 0.000000000000000000, 0.4539904997395412534, 0.8910065241883706744 ) ) ;
#11975 = ADVANCED_FACE ( 'NONE', ( #9502 ), #15315, .T. ) ;
#11976 = ORIENTED_EDGE ( 'NONE', *, *, #1727, .F. ) ;
#11977 = CARTESIAN_POINT ( 'NONE',  ( -0.3562533529037968383, 11.24999999999999467, 23.49729949480461499 ) ) ;
#11978 = CARTESIAN_POINT ( 'NONE',  ( 10.00000000000000000, 50.71018745830443919, 24.33982105418919417 ) ) ;
#11979 = DIRECTION ( 'NONE',  ( 2.031314180040284764E-16, 1.000000000000000000, 1.301042606982601377E-16 ) ) ;
#11980 = DIRECTION ( 'NONE',  ( 1.000000000000000000, 0.000000000000000000, 0.000000000000000000 ) ) ;
#11981 = ORIENTED_EDGE ( 'NONE', *, *, #8885, .T. ) ;
#11982 = DIRECTION ( 'NONE',  ( 1.000000000000000000, 0.000000000000000000, 0.000000000000000000 ) ) ;
#11983 = EDGE_CURVE ( 'NONE', #5722, #538, #10255, .T. ) ;
#11984 = ORIENTED_EDGE ( 'NONE', *, *, #11613, .T. ) ;
#11985 = CYLINDRICAL_SURFACE ( 'NONE', #6346, 24.00000000002399858 ) ;
#11986 = DIRECTION ( 'NONE',  ( -1.000000000000000000, 0.000000000000000000, -0.000000000000000000 ) ) ;
#11987 = ORIENTED_EDGE ( 'NONE', *, *, #18761, .T. ) ;
#11988 = EDGE_CURVE ( 'NONE', #13818, #12293, #18456, .T. ) ;
#11989 = CYLINDRICAL_SURFACE ( 'NONE', #3383, 12.00000000001200817 ) ;
#11990 = VERTEX_POINT ( 'NONE', #1134 ) ;
#11991 = FILL_AREA_STYLE ('',( #6288 ) ) ;
#11992 = CARTESIAN_POINT ( 'NONE',  ( 10.00000000000000000, -23.88582760061464683, -22.76987570971553509 ) ) ;
#11993 = AXIS2_PLACEMENT_3D ( 'NONE', #338, #10786, #12139 ) ;
#11994 = DIRECTION ( 'NONE',  ( 0.000000000000000000, 0.000000000000000000, 1.000000000000000000 ) ) ;
#11995 = DIRECTION ( 'NONE',  ( -0.000000000000000000, 1.000000000000000000, -0.000000000000000000 ) ) ;
#11996 = VECTOR ( 'NONE', #16380, 1000.000000000000000 ) ;
#11997 = DIRECTION ( 'NONE',  ( 0.000000000000000000, 0.000000000000000000, -1.000000000000000000 ) ) ;
#11998 = ORIENTED_EDGE ( 'NONE', *, *, #12370, .F. ) ;
#11999 = DIRECTION ( 'NONE',  ( 0.000000000000000000, -1.000000000000000000, 0.000000000000000000 ) ) ;
#12000 = EDGE_LOOP ( 'NONE', ( #13419, #17633, #14106, #14542 ) ) ;
#12001 = CIRCLE ( 'NONE', #6844, 12.00000000001200462 ) ;
#12002 = DIRECTION ( 'NONE',  ( -1.000000000000000000, 0.000000000000000000, 0.000000000000000000 ) ) ;
#12003 = EDGE_LOOP ( 'NONE', ( #14707, #1913, #9678, #8810 ) ) ;
#12004 = ORIENTED_EDGE ( 'NONE', *, *, #2141, .F. ) ;
#12005 = AXIS2_PLACEMENT_3D ( 'NONE', #4936, #4561, #10738 ) ;
#12006 = ORIENTED_EDGE ( 'NONE', *, *, #13995, .F. ) ;
#12007 = CONICAL_SURFACE ( 'NONE', #14148, 5.560781378645573980, 1.221730476396046816 ) ;
#12008 = CIRCLE ( 'NONE', #8963, 26.24900000002624978 ) ;
#12009 = EDGE_CURVE ( 'NONE', #18400, #3589, #11720, .T. ) ;
#12010 = ADVANCED_FACE ( 'NONE', ( #4792 ), #13471, .T. ) ;
#12011 = EDGE_LOOP ( 'NONE', ( #11309, #4162 ) ) ;
#12012 = DIRECTION ( 'NONE',  ( 1.000000000000000000, 0.000000000000000000, 0.000000000000000000 ) ) ;
#12013 = EDGE_CURVE ( 'NONE', #104, #11956, #802, .T. ) ;
#12014 = EDGE_CURVE ( 'NONE', #7161, #2269, #7606, .T. ) ;
#12015 = SURFACE_STYLE_FILL_AREA ( #16592 ) ;
#12016 = CYLINDRICAL_SURFACE ( 'NONE', #9684, 4.349594641156948605 ) ;
#12017 = CARTESIAN_POINT ( 'NONE',  ( 10.00000000000000000, 0.000000000000000000, 0.000000000000000000 ) ) ;
#12018 = ADVANCED_FACE ( 'NONE', ( #7733 ), #11508, .T. ) ;
#12019 = LINE ( 'NONE', #4693, #8734 ) ;
#12020 = CARTESIAN_POINT ( 'NONE',  ( 0.000000000000000000, -55.51919907100660367, 9.823366686500467182 ) ) ;
#12021 = AXIS2_PLACEMENT_3D ( 'NONE', #15388, #8161, #3873 ) ;
#12022 = LINE ( 'NONE', #7107, #8374 ) ;
#12023 = CARTESIAN_POINT ( 'NONE',  ( 0.6666666666666658525, -4.233901974057276085, -3.300726591567086476 ) ) ;
#12024 = EDGE_LOOP ( 'NONE', ( #15316, #17828, #7651, #18352 ) ) ;
#12025 = CYLINDRICAL_SURFACE ( 'NONE', #17228, 12.00000000001200462 ) ;
#12026 = FACE_OUTER_BOUND ( 'NONE', #10676, .T. ) ;
#12027 = EDGE_CURVE ( 'NONE', #13113, #912, #2907, .T. ) ;
#12028 = DIRECTION ( 'NONE',  ( -0.000000000000000000, 1.000000000000000000, -0.000000000000000000 ) ) ;
#12029 = VERTEX_POINT ( 'NONE', #8971 ) ;
#12030 = ORIENTED_EDGE ( 'NONE', *, *, #17418, .F. ) ;
#12031 = VECTOR ( 'NONE', #4770, 1000.000000000000000 ) ;
#12032 = CARTESIAN_POINT ( 'NONE',  ( 10.00000000000000000, 62.72529079327814117, -5.876895005581764586 ) ) ;
#12033 = CARTESIAN_POINT ( 'NONE',  ( -117.1020693116506379, -25.00000000000000000, -19.69080595179801207 ) ) ;
#12034 = EDGE_CURVE ( 'NONE', #10765, #4921, #12022, .T. ) ;
#12035 = CYLINDRICAL_SURFACE ( 'NONE', #14366, 24.00000000002400213 ) ;
#12036 = EDGE_LOOP ( 'NONE', ( #16622, #5964 ) ) ;
#12037 = CIRCLE ( 'NONE', #13269, 30.00000000000000000 ) ;
#12038 = CONICAL_SURFACE ( 'NONE', #16302, 2.059999999999998721, 0.9599310885968738161 ) ;
#12039 = EDGE_CURVE ( 'NONE', #10957, #514, #12008, .T. ) ;
#12040 = AXIS2_PLACEMENT_3D ( 'NONE', #16990, #5350, #11055 ) ;
#12041 = DIRECTION ( 'NONE',  ( -1.000000000000000000, 0.000000000000000000, 0.000000000000000000 ) ) ;
#12042 = DIRECTION ( 'NONE',  ( -1.000000000000000000, -0.000000000000000000, 0.000000000000000000 ) ) ;
#12043 = CIRCLE ( 'NONE', #11440, 2.649999999999999467 ) ;
#12044 = CIRCLE ( 'NONE', #12363, 33.00000000003299760 ) ;
#12046 = AXIS2_PLACEMENT_3D ( 'NONE', #15821, #2770, #14384 ) ;
#12045 = CARTESIAN_POINT ( 'NONE',  ( 0.000000000000000000, 1.178949249685212974, -2.042000000000001148 ) ) ;
#12047 = ORIENTED_EDGE ( 'NONE', *, *, #13378, .F. ) ;
#12048 = CARTESIAN_POINT ( 'NONE',  ( 10.00000000000000000, 40.58063702438344933, 39.14194549634378006 ) ) ;
#12049 = VERTEX_POINT ( 'NONE', #11935 ) ;
#12050 = CARTESIAN_POINT ( 'NONE',  ( 0.000000000000000000, 0.000000000000000000, 0.000000000000000000 ) ) ;
#12051 = VERTEX_POINT ( 'NONE', #14793 ) ;
#12052 = EDGE_CURVE ( 'NONE', #16334, #4819, #7759, .T. ) ;
#12053 = FACE_OUTER_BOUND ( 'NONE', #7101, .T. ) ;
#12054 = CARTESIAN_POINT ( 'NONE',  ( -4.141042297810615835, 2.227970268150415656, -3.687027686973619822 ) ) ;
#12055 = CIRCLE ( 'NONE', #10241, 56.24900000005625600 ) ;
#12056 = VERTEX_POINT ( 'NONE', #17220 ) ;
#12057 = ORIENTED_EDGE ( 'NONE', *, *, #780, .F. ) ;
#12058 = AXIS2_PLACEMENT_3D ( 'NONE', #13895, #12364, #9703 ) ;
#12059 = CARTESIAN_POINT ( 'NONE',  ( 10.00000000000000000, 0.000000000000000000, 0.000000000000000000 ) ) ;
#12060 =( NAMED_UNIT ( * ) SI_UNIT ( $, .STERADIAN. ) SOLID_ANGLE_UNIT ( ) );
#12061 = CIRCLE ( 'NONE', #14811, 2.649999999999999467 ) ;
#12062 = EDGE_LOOP ( 'NONE', ( #3691, #9586, #3731, #17093 ) ) ;
#12063 = DIRECTION ( 'NONE',  ( -1.000000000000000000, 0.000000000000000000, 0.000000000000000000 ) ) ;
#12064 = AXIS2_PLACEMENT_3D ( 'NONE', #2208, #4964, #12496 ) ;
#12065 = AXIS2_PLACEMENT_3D ( 'NONE', #3531, #877, #16962 ) ;
#12066 = LINE ( 'NONE', #1969, #450 ) ;
#12067 = CIRCLE ( 'NONE', #14809, 30.00000000000000000 ) ;
#12068 = VERTEX_POINT ( 'NONE', #13277 ) ;
#12069 = AXIS2_PLACEMENT_3D ( 'NONE', #1339, #7129, #5896 ) ;
#12070 = AXIS2_PLACEMENT_3D ( 'NONE', #6926, #1026, #11209 ) ;
#12071 = ORIENTED_EDGE ( 'NONE', *, *, #4822, .T. ) ;
#12072 = DIRECTION ( 'NONE',  ( -1.000000000000000000, -0.000000000000000000, -0.000000000000000000 ) ) ;
#12073 = VECTOR ( 'NONE', #13379, 1000.000000000000000 ) ;
#12074 = CARTESIAN_POINT ( 'NONE',  ( 2.500000000000000000, 2.357898499370431722, -2.818925648462311528E-15 ) ) ;
#12075 = CARTESIAN_POINT ( 'NONE',  ( -26.29305231718568336, -26.50000000000000000, -19.10302069950552095 ) ) ;
#12076 = VERTEX_POINT ( 'NONE', #14439 ) ;
#12077 = CARTESIAN_POINT ( 'NONE',  ( 10.04305231718579705, -26.50000000000000000, 33.55933677959249195 ) ) ;
#12078 = EDGE_CURVE ( 'NONE', #14399, #980, #9978, .T. ) ;
#12079 = CARTESIAN_POINT ( 'NONE',  ( 0.000000000000000000, 1.305124410222461284, -2.000000000000000000 ) ) ;
#12080 = CARTESIAN_POINT ( 'NONE',  ( 0.000000000000000000, -26.50000000000000000, 0.000000000000000000 ) ) ;
#12081 = CARTESIAN_POINT ( 'NONE',  ( 34.55500000000001393, 0.000000000000000000, 2.500000000000000888 ) ) ;
#12082 = ORIENTED_EDGE ( 'NONE', *, *, #1352, .F. ) ;
#12083 = DIRECTION ( 'NONE',  ( -1.000000000000000000, 0.000000000000000000, 0.000000000000000000 ) ) ;
#12084 = DIRECTION ( 'NONE',  ( -1.000000000000000000, -0.000000000000000000, -0.000000000000000000 ) ) ;
#12085 = ORIENTED_EDGE ( 'NONE', *, *, #12277, .T. ) ;
#12086 = CARTESIAN_POINT ( 'NONE',  ( 5.000000000000000888, 4.250000000000000000, 0.000000000000000000 ) ) ;
#12087 = CARTESIAN_POINT ( 'NONE',  ( -26.29305231718584324, -30.00000000000000000, 19.10302069950530779 ) ) ;
#12088 = AXIS2_PLACEMENT_3D ( 'NONE', #1606, #7410, #14461 ) ;
#12089 = AXIS2_PLACEMENT_3D ( 'NONE', #4045, #11364, #5650 ) ;
#12090 = AXIS2_PLACEMENT_3D ( 'NONE', #14532, #7948, #17955 ) ;
#12091 = AXIS2_PLACEMENT_3D ( 'NONE', #6007, #1544, #18689 ) ;
#12092 = EDGE_CURVE ( 'NONE', #14358, #407, #17746, .T. ) ;
#12093 = VERTEX_POINT ( 'NONE', #11848 ) ;
#12094 = EDGE_CURVE ( 'NONE', #16857, #11035, #473, .T. ) ;
#12095 = CARTESIAN_POINT ( 'NONE',  ( 10.00000000000000000, -14.19907017806883864, 22.07705612348834734 ) ) ;
#12096 = ORIENTED_EDGE ( 'NONE', *, *, #14553, .F. ) ;
#12097 = DIRECTION ( 'NONE',  ( 0.000000000000000000, 0.000000000000000000, 1.000000000000000000 ) ) ;
#12098 = AXIS2_PLACEMENT_3D ( 'NONE', #2395, #16973, #5150 ) ;
#12099 = CARTESIAN_POINT ( 'NONE',  ( 5.000000000000004441, 0.000000000000000000, 0.000000000000000000 ) ) ;
#12100 = DIRECTION ( 'NONE',  ( 0.000000000000000000, 0.000000000000000000, 1.000000000000000000 ) ) ;
#12101 = AXIS2_PLACEMENT_3D ( 'NONE', #600, #16501, #4690 ) ;
#12102 = DIRECTION ( 'NONE',  ( -1.000000000000000000, 0.000000000000000000, 0.000000000000000000 ) ) ;
#12103 = EDGE_LOOP ( 'NONE', ( #17705, #5213, #15367, #2552, #18143 ) ) ;
#12104 = CIRCLE ( 'NONE', #12424, 4.250000000000000000 ) ;
#12105 = CARTESIAN_POINT ( 'NONE',  ( 10.00000000000000000, -61.03368945066424089, -15.61693798565562119 ) ) ;
#12106 = PRODUCT_DEFINITION_SHAPE ( 'NONE', 'NONE',  #18833 ) ;
#12107 = CARTESIAN_POINT ( 'NONE',  ( -4.000000000000000000, 2.309401076758498483, -3.433295621305379353 ) ) ;
#12108 = ORIENTED_EDGE ( 'NONE', *, *, #3902, .F. ) ;
#12109 = ORIENTED_EDGE ( 'NONE', *, *, #4945, .T. ) ;
#12110 = AXIS2_PLACEMENT_3D ( 'NONE', #18144, #18335, #10907 ) ;
#12111 = AXIS2_PLACEMENT_3D ( 'NONE', #9909, #15728, #2680 ) ;
#12112 = ORIENTED_EDGE ( 'NONE', *, *, #11389, .T. ) ;
#12113 = AXIS2_PLACEMENT_3D ( 'NONE', #6697, #6595, #11158 ) ;
#12114 = VECTOR ( 'NONE', #9413, 1000.000000000000000 ) ;
#12115 = ORIENTED_EDGE ( 'NONE', *, *, #6426, .F. ) ;
#12116 = CARTESIAN_POINT ( 'NONE',  ( 0.000000000000000000, -13.40641754777648487, -24.79895094899273644 ) ) ;
#12117 = DIRECTION ( 'NONE',  ( 0.000000000000000000, 0.000000000000000000, 1.000000000000000000 ) ) ;
#12118 = CARTESIAN_POINT ( 'NONE',  ( 0.000000000000000000, -22.76987570971544272, 23.88582760061473209 ) ) ;
#12119 = DIRECTION ( 'NONE',  ( -1.000000000000000000, 0.000000000000000000, 0.000000000000000000 ) ) ;
#12120 = CARTESIAN_POINT ( 'NONE',  ( 0.000000000000000000, 41.62350880771921169, 47.29147401531970019 ) ) ;
#12121 = CARTESIAN_POINT ( 'NONE',  ( -10.00000000000000000, -5.120903701083534543E-13, -45.00000000000000000 ) ) ;
#12122 = AXIS2_PLACEMENT_3D ( 'NONE', #17468, #6906, #8703 ) ;
#12123 = CYLINDRICAL_SURFACE ( 'NONE', #18015, 33.00000000003299760 ) ;
#12124 = CARTESIAN_POINT ( 'NONE',  ( -117.1020693116506379, -34.99999999999999289, -19.69080595179801207 ) ) ;
#12125 = ORIENTED_EDGE ( 'NONE', *, *, #3429, .F. ) ;
#12126 = CARTESIAN_POINT ( 'NONE',  ( 10.00000000000000000, 24.46385708179984064, 9.514709542736980552 ) ) ;
#12127 = VERTEX_POINT ( 'NONE', #4273 ) ;
#12128 = AXIS2_PLACEMENT_3D ( 'NONE', #2657, #12853, #1145 ) ;
#12129 = LINE ( 'NONE', #12221, #10517 ) ;
#12130 = DIRECTION ( 'NONE',  ( -1.000000000000000000, 0.000000000000000000, 0.000000000000000000 ) ) ;
#12131 = DIRECTION ( 'NONE',  ( -0.000000000000000000, 1.000000000000000000, -0.000000000000000000 ) ) ;
#12132 = VECTOR ( 'NONE', #2102, 1000.000000000000000 ) ;
#12133 = ORIENTED_EDGE ( 'NONE', *, *, #17486, .F. ) ;
#12134 = ORIENTED_EDGE ( 'NONE', *, *, #7274, .T. ) ;
#12135 = AXIS2_PLACEMENT_3D ( 'NONE', #15968, #14360, #8729 ) ;
#12136 = EDGE_CURVE ( 'NONE', #7040, #17682, #8547, .T. ) ;
#12137 = ADVANCED_FACE ( 'NONE', ( #16319 ), #18732, .T. ) ;
#12138 = DIRECTION ( 'NONE',  ( 1.000000000000000000, 0.000000000000000000, -0.000000000000000000 ) ) ;
#12139 = DIRECTION ( 'NONE',  ( 6.123233995736766036E-17, -1.000000000000000000, 0.000000000000000000 ) ) ;
#12141 = ADVANCED_FACE ( 'NONE', ( #10414 ), #13381, .T. ) ;
#12140 = DIRECTION ( 'NONE',  ( 0.000000000000000000, 0.000000000000000000, 1.000000000000000000 ) ) ;
#12142 = ORIENTED_EDGE ( 'NONE', *, *, #2115, .T. ) ;
#12143 = EDGE_CURVE ( 'NONE', #13712, #12930, #15186, .T. ) ;
#12144 = AXIS2_PLACEMENT_3D ( 'NONE', #14681, #14771, #10208 ) ;
#12145 = VECTOR ( 'NONE', #16830, 1000.000000000000000 ) ;
#12146 = ADVANCED_FACE ( 'NONE', ( #9259 ), #606, .T. ) ;
#12147 = CARTESIAN_POINT ( 'NONE',  ( -10.00000000000000000, 0.000000000000000000, 0.000000000000000000 ) ) ;
#12148 = DIRECTION ( 'NONE',  ( 0.000000000000000000, 0.8090169943749446757, 0.5877852522924769119 ) ) ;
#12149 = CARTESIAN_POINT ( 'NONE',  ( -10.00000000000000000, 42.79754323328179311, -13.90576474687299680 ) ) ;
#12150 = ORIENTED_EDGE ( 'NONE', *, *, #9778, .T. ) ;
#12151 = DIRECTION ( 'NONE',  ( 0.000000000000000000, -0.3090169943749548342, 0.9510565162951511997 ) ) ;
#12152 = ADVANCED_FACE ( 'NONE', ( #10776 ), #16598, .T. ) ;
#12153 = ORIENTED_EDGE ( 'NONE', *, *, #541, .T. ) ;
#12154 = CARTESIAN_POINT ( 'NONE',  ( 10.00000000000000000, 24.79895094899259789, -13.40641754777674421 ) ) ;
#12155 = ORIENTED_EDGE ( 'NONE', *, *, #6534, .T. ) ;
#12156 = FACE_OUTER_BOUND ( 'NONE', #8546, .T. ) ;
#12157 = CARTESIAN_POINT ( 'NONE',  ( 0.000000000000000000, -57.83923611457302627, -24.97244012287563919 ) ) ;
#12158 = AXIS2_PLACEMENT_3D ( 'NONE', #12288, #7914, #12198 ) ;
#12159 = EDGE_LOOP ( 'NONE', ( #7436, #782, #2700, #16391 ) ) ;
#12160 = EDGE_LOOP ( 'NONE', ( #9879, #8743, #16496, #738 ) ) ;
#12161 = EDGE_CURVE ( 'NONE', #12340, #3488, #10791, .T. ) ;
#12162 = DIRECTION ( 'NONE',  ( 0.000000000000000000, -0.8090169943749530024, 0.5877852522924653655 ) ) ;
#12163 = CIRCLE ( 'NONE', #17355, 33.00000000003299760 ) ;
#12164 = SHAPE_REPRESENTATION_RELATIONSHIP ( 'NONE' , 'NONE' ,  #434, #4227 ) ;
#12165 = ADVANCED_FACE ( 'NONE', ( #13746 ), #7838, .T. ) ;
#12166 = VERTEX_POINT ( 'NONE', #5170 ) ;
#12167 = CARTESIAN_POINT ( 'NONE',  ( 5.000000000000002665, 3.306546357697854226E-16, 2.700000000000000622 ) ) ;
#12168 = EDGE_CURVE ( 'NONE', #11128, #10830, #5008, .T. ) ;
#12169 = CARTESIAN_POINT ( 'NONE',  ( -4.101948962586059011, 2.368261337751163875, -3.681124513963739187 ) ) ;
#12170 = VECTOR ( 'NONE', #5197, 999.9999999999998863 ) ;
#12171 = CIRCLE ( 'NONE', #16171, 63.00000000006298961 ) ;
#12172 = APPLICATION_CONTEXT ( 'automotive_design' ) ;
#12173 = VERTEX_POINT ( 'NONE', #797 ) ;
#12174 = CIRCLE ( 'NONE', #602, 2.055000000000000160 ) ;
#12175 = ORIENTED_EDGE ( 'NONE', *, *, #53, .T. ) ;
#12176 = DIRECTION ( 'NONE',  ( -0.000000000000000000, 1.000000000000000000, -0.000000000000000000 ) ) ;
#12177 = CARTESIAN_POINT ( 'NONE',  ( -0.3562533529037968383, 13.24999999999999467, 23.49729949480461499 ) ) ;
#12178 = DIRECTION ( 'NONE',  ( 1.000000000000000000, 0.000000000000000000, 0.000000000000000000 ) ) ;
#12179 = ORIENTED_EDGE ( 'NONE', *, *, #13205, .F. ) ;
#12180 = CARTESIAN_POINT ( 'NONE',  ( 0.000000000000000000, 4.769696007084728073, 1.500000000000000000 ) ) ;
#12181 = CARTESIAN_POINT ( 'NONE',  ( 10.00000000000000000, 25.42247726998032320, -12.18267823974723640 ) ) ;
#12182 = DIRECTION ( 'NONE',  ( 0.000000000000000000, -1.000000000000000000, 0.000000000000000000 ) ) ;
#12183 = DIRECTION ( 'NONE',  ( 0.000000000000000000, 0.000000000000000000, 1.000000000000000000 ) ) ;
#12184 = ORIENTED_EDGE ( 'NONE', *, *, #1904, .T. ) ;
#12185 =( NAMED_UNIT ( * ) SI_UNIT ( $, .STERADIAN. ) SOLID_ANGLE_UNIT ( ) );
#12186 = ORIENTED_EDGE ( 'NONE', *, *, #8076, .T. ) ;
#12187 = DIRECTION ( 'NONE',  ( 0.000000000000000000, 0.000000000000000000, -1.000000000000000000 ) ) ;
#12188 = FACE_OUTER_BOUND ( 'NONE', #5372, .T. ) ;
#12189 = EDGE_CURVE ( 'NONE', #9984, #3645, #9543, .T. ) ;
#12190 = ORIENTED_EDGE ( 'NONE', *, *, #13445, .F. ) ;
#12191 = VERTEX_POINT ( 'NONE', #3565 ) ;
#12192 = CARTESIAN_POINT ( 'NONE',  ( 10.00000000000000000, 10.11537145609375798, 55.33199130079789541 ) ) ;
#12193 = DIRECTION ( 'NONE',  ( -1.000000000000000000, 0.000000000000000000, 0.000000000000000000 ) ) ;
#12194 = CARTESIAN_POINT ( 'NONE',  ( 10.00000000000000000, -27.72801475327278453, -5.086963483077506787 ) ) ;
#12195 = DIRECTION ( 'NONE',  ( -1.000000000000000000, 0.000000000000000000, 0.000000000000000000 ) ) ;
#12196 = DIRECTION ( 'NONE',  ( 0.000000000000000000, -1.224646799147353454E-16, 1.000000000000000000 ) ) ;
#12197 = ORIENTED_EDGE ( 'NONE', *, *, #1777, .T. ) ;
#12198 = DIRECTION ( 'NONE',  ( 0.000000000000000000, -0.8090169943749531134, 0.5877852522924653655 ) ) ;
#12199 = EDGE_CURVE ( 'NONE', #6003, #11692, #9284, .T. ) ;
#12200 = DIRECTION ( 'NONE',  ( -1.000000000000000000, 0.000000000000000000, 0.000000000000000000 ) ) ;
#12201 = ORIENTED_EDGE ( 'NONE', *, *, #14933, .F. ) ;
#12202 = CONTEXT_DEPENDENT_SHAPE_REPRESENTATION ( #14268, #4344 ) ;
#12203 = EDGE_CURVE ( 'NONE', #14748, #1691, #7447, .T. ) ;
#12204 = VERTEX_POINT ( 'NONE', #2125 ) ;
#12205 = AXIS2_PLACEMENT_3D ( 'NONE', #10527, #14631, #8998 ) ;
#12206 = ORIENTED_EDGE ( 'NONE', *, *, #9515, .T. ) ;
#12207 = ORIENTED_EDGE ( 'NONE', *, *, #15174, .F. ) ;
#12209 = DIRECTION ( 'NONE',  ( 0.000000000000000000, 0.000000000000000000, 1.000000000000000000 ) ) ;
#12208 = AXIS2_PLACEMENT_3D ( 'NONE', #13449, #390, #1911 ) ;
#12210 = CARTESIAN_POINT ( 'NONE',  ( 0.000000000000000000, 0.5192545390863916310, 0.000000000000000000 ) ) ;
#12211 = CYLINDRICAL_SURFACE ( 'NONE', #6931, 4.250000000000000000 ) ;
#12212 = DIRECTION ( 'NONE',  ( 0.000000000000000000, 0.000000000000000000, 1.000000000000000000 ) ) ;
#12213 = DIRECTION ( 'NONE',  ( 0.000000000000000000, 0.9510565162951544194, -0.3090169943749447312 ) ) ;
#12214 = DIRECTION ( 'NONE',  ( -1.000000000000000000, 0.000000000000000000, -0.000000000000000000 ) ) ;
#12215 = CARTESIAN_POINT ( 'NONE',  ( 10.00000000000000000, 12.18267823974751352, 25.42247726998019530 ) ) ;
#12216 = CARTESIAN_POINT ( 'NONE',  ( 0.000000000000000000, -16.45250512421895550, 53.92768374110886498 ) ) ;
#12217 = ORIENTED_EDGE ( 'NONE', *, *, #11214, .F. ) ;
#12218 = CARTESIAN_POINT ( 'NONE',  ( 10.00000000000000000, 18.38754094778241210, 53.29895248911682870 ) ) ;
#12219 = ORIENTED_EDGE ( 'NONE', *, *, #8560, .F. ) ;
#12220 = ADVANCED_FACE ( 'NONE', ( #15082 ), #8678, .T. ) ;
#12221 = CARTESIAN_POINT ( 'NONE',  ( -1.128893538851230005, 11.24999999999999467, 23.47286943213250154 ) ) ;
#12222 = CYLINDRICAL_SURFACE ( 'NONE', #18042, 28.00000000000000355 ) ;
#12223 = DIRECTION ( 'NONE',  ( 0.000000000000000000, 0.000000000000000000, -1.000000000000000000 ) ) ;
#12224 = ORIENTED_EDGE ( 'NONE', *, *, #15873, .F. ) ;
#12225 = ORIENTED_EDGE ( 'NONE', *, *, #16510, .F. ) ;
#12226 = DIRECTION ( 'NONE',  ( -1.000000000000000000, 0.000000000000000000, -0.000000000000000000 ) ) ;
#12227 = DIRECTION ( 'NONE',  ( -0.06790287765481992088, 0.000000000000000000, 0.9976919360234375311 ) ) ;
#12228 = DIRECTION ( 'NONE',  ( -1.000000000000000000, 0.000000000000000000, 0.000000000000000000 ) ) ;
#12229 = ORIENTED_EDGE ( 'NONE', *, *, #8616, .T. ) ;
#12230 = DIRECTION ( 'NONE',  ( -1.000000000000000000, 0.000000000000000000, 0.000000000000000000 ) ) ;
#12231 = LINE ( 'NONE', #6428, #11859 ) ;
#12232 = DIRECTION ( 'NONE',  ( 0.000000000000000000, 0.000000000000000000, 1.000000000000000000 ) ) ;
#12233 = ORIENTED_EDGE ( 'NONE', *, *, #14121, .F. ) ;
#12234 = EDGE_CURVE ( 'NONE', #16305, #17232, #2034, .T. ) ;
#12235 = CARTESIAN_POINT ( 'NONE',  ( 10.04305231718605285, -26.50000000000000000, -33.55933677959240669 ) ) ;
#12236 = AXIS2_PLACEMENT_3D ( 'NONE', #857, #15512, #12466 ) ;
#12237 = EDGE_CURVE ( 'NONE', #18322, #8760, #7154, .T. ) ;
#12238 = VECTOR ( 'NONE', #14613, 1000.000000000000114 ) ;
#12239 = VERTEX_POINT ( 'NONE', #4972 ) ;
#12240 = UNCERTAINTY_MEASURE_WITH_UNIT (LENGTH_MEASURE( 1.000000000000000082E-05 ), #2210, 'distance_accuracy_value', 'NONE');
#12241 = CYLINDRICAL_SURFACE ( 'NONE', #11188, 30.00000000000000000 ) ;
#12242 = VERTEX_POINT ( 'NONE', #2414 ) ;
#12243 = PRODUCT_DEFINITION ( 'UNKNOWN', '', #5004, #16068 ) ;
#12244 = FACE_OUTER_BOUND ( 'NONE', #9176, .T. ) ;
#12245 = CARTESIAN_POINT ( 'NONE',  ( -3.436319922987618902, 2.634841920961291439, -3.531542292955721862 ) ) ;
#12246 = ORIENTED_EDGE ( 'NONE', *, *, #17614, .T. ) ;
#12247 = ORIENTED_EDGE ( 'NONE', *, *, #14933, .T. ) ;
#12248 = DIRECTION ( 'NONE',  ( 0.000000000000000000, 0.8090169943749486725, -0.5877852522924713607 ) ) ;
#12249 = EDGE_LOOP ( 'NONE', ( #11239, #17264, #6101, #8064 ) ) ;
#12250 = CYLINDRICAL_SURFACE ( 'NONE', #2428, 27.00000000000000355 ) ;
#12251 = CIRCLE ( 'NONE', #5262, 0.2000000000000000944 ) ;
#12252 = EDGE_CURVE ( 'NONE', #6907, #6265, #5071, .T. ) ;
#12253 = CIRCLE ( 'NONE', #7385, 2.649999999999995914 ) ;
#12254 = DIRECTION ( 'NONE',  ( -1.000000000000000000, 0.000000000000000000, -0.000000000000000000 ) ) ;
#12255 = LINE ( 'NONE', #651, #2651 ) ;
#12256 = ORIENTED_EDGE ( 'NONE', *, *, #12394, .T. ) ;
#12257 = EDGE_CURVE ( 'NONE', #10765, #15213, #3501, .T. ) ;
#12258 = ADVANCED_FACE ( 'NONE', ( #700 ), #6502, .T. ) ;
#12259 = PRODUCT_DEFINITION_SHAPE ( 'NONE', 'NONE',  #18829 ) ;
#12260 = ORIENTED_EDGE ( 'NONE', *, *, #5154, .T. ) ;
#12261 = DIRECTION ( 'NONE',  ( -0.000000000000000000, 1.000000000000000000, -0.000000000000000000 ) ) ;
#12262 = CARTESIAN_POINT ( 'NONE',  ( 10.00000000000000000, 26.45033635316149301, 33.75576474687247241 ) ) ;
#12263 = DIRECTION ( 'NONE',  ( -1.000000000000000000, 0.000000000000000000, -0.000000000000000000 ) ) ;
#12264 = VERTEX_POINT ( 'NONE', #8020 ) ;
#12265 = CARTESIAN_POINT ( 'NONE',  ( 10.00000000000000000, -5.086963483077008519, -27.72801475327286980 ) ) ;
#12266 = AXIS2_PLACEMENT_3D ( 'NONE', #17944, #13282, #17846 ) ;
#12267 = EDGE_CURVE ( 'NONE', #15559, #17515, #13830, .T. ) ;
#12268 = DIRECTION ( 'NONE',  ( 0.000000000000000000, 1.000000000000000000, 0.000000000000000000 ) ) ;
#12269 = CYLINDRICAL_SURFACE ( 'NONE', #7985, 24.00000000002399858 ) ;
#12270 = CARTESIAN_POINT ( 'NONE',  ( 2.250000000000000000, -27.60846790388774608, -2.000000000000000000 ) ) ;
#12271 = EDGE_LOOP ( 'NONE', ( #4929, #8955 ) ) ;
#12272 = EDGE_CURVE ( 'NONE', #3012, #8916, #6859, .T. ) ;
#12273 = DIRECTION ( 'NONE',  ( -1.000000000000000000, 0.000000000000000000, 0.000000000000000000 ) ) ;
#12274 = ORIENTED_EDGE ( 'NONE', *, *, #1863, .T. ) ;
#12275 = CARTESIAN_POINT ( 'NONE',  ( 10.00000000000000000, -14.27431201565505070, -29.75305054077486488 ) ) ;
#12276 = CARTESIAN_POINT ( 'NONE',  ( 0.9999999999999997780, -27.60846790388774608, -2.000000000000000000 ) ) ;
#12277 = EDGE_CURVE ( 'NONE', #12626, #4026, #1276, .T. ) ;
#12278 =( GEOMETRIC_REPRESENTATION_CONTEXT ( 3 ) GLOBAL_UNCERTAINTY_ASSIGNED_CONTEXT ( ( #3680 ) ) GLOBAL_UNIT_ASSIGNED_CONTEXT ( ( #8870, #16493, #3449 ) ) REPRESENTATION_CONTEXT ( 'NONE', 'WORKASPACE' ) );
#12279 = ORIENTED_EDGE ( 'NONE', *, *, #17063, .F. ) ;
#12280 = ORIENTED_EDGE ( 'NONE', *, *, #1469, .F. ) ;
#12281 = DIRECTION ( 'NONE',  ( 1.000000000000000000, 0.000000000000000000, 0.000000000000000000 ) ) ;
#12282 = CARTESIAN_POINT ( 'NONE',  ( 4.000000000000000000, 2.512223110932545023, -3.469391141908803711 ) ) ;
#12283 = DIRECTION ( 'NONE',  ( -1.000000000000000000, -0.000000000000000000, -0.000000000000000000 ) ) ;
#12284 = CARTESIAN_POINT ( 'NONE',  ( 4.999999999999999112, 13.79392154159224404, -61.47135697633764551 ) ) ;
#12285 = LINE ( 'NONE', #10670, #4500 ) ;
#12286 = CARTESIAN_POINT ( 'NONE',  ( 5.384454397937118664, 0.000000000000000000, -4.484454397937119197 ) ) ;
#12287 = ORIENTED_EDGE ( 'NONE', *, *, #764, .T. ) ;
#12288 = CARTESIAN_POINT ( 'NONE',  ( 0.000000000000000000, 0.000000000000000000, 0.000000000000000000 ) ) ;
#12289 = EDGE_CURVE ( 'NONE', #6455, #9337, #18792, .T. ) ;
#12290 = SURFACE_SIDE_STYLE ('',( #11407 ) ) ;
#12291 = CARTESIAN_POINT ( 'NONE',  ( -4.000000000000000000, -1.942223658245633811, -0.3516579909967644246 ) ) ;
#12292 = VERTEX_POINT ( 'NONE', #17176 ) ;
#12293 = VERTEX_POINT ( 'NONE', #18691 ) ;
#12294 = ORIENTED_EDGE ( 'NONE', *, *, #14586, .F. ) ;
#12295 = EDGE_LOOP ( 'NONE', ( #9110, #10974, #6660, #1547 ) ) ;
#12296 = COLOUR_RGB ( '',1.000000000000000000, 0.9490196078431372140, 0.9098039215686274384 ) ;
#12297 = DIRECTION ( 'NONE',  ( 0.000000000000000000, 0.000000000000000000, -1.000000000000000000 ) ) ;
#12298 = DIRECTION ( 'NONE',  ( 0.000000000000000000, 0.000000000000000000, 1.000000000000000000 ) ) ;
#12299 = AXIS2_PLACEMENT_3D ( 'NONE', #15226, #1227, #5413 ) ;
#12300 = CYLINDRICAL_SURFACE ( 'NONE', #6884, 33.00000000003299760 ) ;
#12301 = DIRECTION ( 'NONE',  ( 0.000000000000000000, 0.000000000000000000, -1.000000000000000000 ) ) ;
#12302 = DIRECTION ( 'NONE',  ( -1.000000000000000000, -0.000000000000000000, -0.000000000000000000 ) ) ;
#12303 = DIRECTION ( 'NONE',  ( -1.000000000000000000, 0.000000000000000000, 0.000000000000000000 ) ) ;
#12304 = CARTESIAN_POINT ( 'NONE',  ( 3.309651814758565180, -5.455921364805393026, -1.000000000000000000 ) ) ;
#12305 = ORIENTED_EDGE ( 'NONE', *, *, #12277, .F. ) ;
#12306 = CARTESIAN_POINT ( 'NONE',  ( -79.64793068852927149, -34.99999999999999289, 31.86039329588764701 ) ) ;
#12307 = EDGE_LOOP ( 'NONE', ( #15691, #3373, #688, #15545 ) ) ;
#12308 = ADVANCED_FACE ( 'NONE', ( #14117 ), #14150, .T. ) ;
#12309 = DIRECTION ( 'NONE',  ( 0.000000000000000000, 0.000000000000000000, 1.000000000000000000 ) ) ;
#12310 = FACE_OUTER_BOUND ( 'NONE', #12476, .T. ) ;
#12311 = VERTEX_POINT ( 'NONE', #18397 ) ;
#12312 = EDGE_LOOP ( 'NONE', ( #17422, #7490 ) ) ;
#12313 = DIRECTION ( 'NONE',  ( 0.000000000000000000, 0.000000000000000000, 1.000000000000000000 ) ) ;
#12314 = DIRECTION ( 'NONE',  ( 6.123233995736766036E-17, -1.000000000000000000, 0.000000000000000000 ) ) ;
#12315 = ORIENTED_EDGE ( 'NONE', *, *, #6683, .F. ) ;
#12316 = FACE_OUTER_BOUND ( 'NONE', #4753, .T. ) ;
#12317 = EDGE_LOOP ( 'NONE', ( #18474, #10483 ) ) ;
#12318 = VECTOR ( 'NONE', #10429, 1000.000000000000000 ) ;
#12319 = VECTOR ( 'NONE', #8229, 1000.000000000000000 ) ;
#12320 = B_SPLINE_CURVE_WITH_KNOTS ( 'NONE', 3,
 ( #12872, #8296, #14096, #8485, #7133, #16865 ),
 .UNSPECIFIED., .F., .F.,
 ( 4, 2, 4 ),
 ( 4.336808689942017736E-19, 0.0002095117440864781224, 0.0004190234881729558111 ),
 .UNSPECIFIED. ) ;
#12321 = EDGE_CURVE ( 'NONE', #16631, #8012, #7069, .T. ) ;
#12322 = DIRECTION ( 'NONE',  ( -1.000000000000000000, 0.000000000000000000, 0.000000000000000000 ) ) ;
#12323 = DIRECTION ( 'NONE',  ( 0.000000000000000000, 1.000000000000000000, 0.000000000000000000 ) ) ;
#12324 = VECTOR ( 'NONE', #15701, 1000.000000000000000 ) ;
#12325 = LINE ( 'NONE', #6902, #11181 ) ;
#12326 = ORIENTED_EDGE ( 'NONE', *, *, #935, .F. ) ;
#12327 = DIRECTION ( 'NONE',  ( 0.000000000000000000, 0.000000000000000000, 1.000000000000000000 ) ) ;
#12328 = EDGE_CURVE ( 'NONE', #3677, #14362, #9893, .T. ) ;
#12329 = AXIS2_PLACEMENT_3D ( 'NONE', #7750, #16436, #3294 ) ;
#12330 = ORIENTED_EDGE ( 'NONE', *, *, #8375, .F. ) ;
#12331 = CARTESIAN_POINT ( 'NONE',  ( 10.00000000000000000, 10.11537145609375798, 55.33199130079789541 ) ) ;
#12332 = VECTOR ( 'NONE', #586, 1000.000000000000000 ) ;
#12333 = ORIENTED_EDGE ( 'NONE', *, *, #7870, .F. ) ;
#12334 = LINE ( 'NONE', #18147, #4750 ) ;
#12335 = DIRECTION ( 'NONE',  ( 0.000000000000000000, 0.000000000000000000, 1.000000000000000000 ) ) ;
#12336 = ORIENTED_EDGE ( 'NONE', *, *, #2704, .T. ) ;
#12337 = ORIENTED_EDGE ( 'NONE', *, *, #6205, .T. ) ;
#12338 = LINE ( 'NONE', #2532, #12650 ) ;
#12339 = PRESENTATION_STYLE_ASSIGNMENT (( #6531 ) ) ;
#12340 = VERTEX_POINT ( 'NONE', #14032 ) ;
#12341 = CARTESIAN_POINT ( 'NONE',  ( -79.64793068852927149, -30.00000000000000000, 31.86039329588764701 ) ) ;
#12342 = AXIS2_PLACEMENT_3D ( 'NONE', #11491, #18539, #5676 ) ;
#12343 = CIRCLE ( 'NONE', #13577, 12.00000000001200462 ) ;
#12344 = AXIS2_PLACEMENT_3D ( 'NONE', #224, #4784, #2021 ) ;
#12345 = VECTOR ( 'NONE', #15535, 1000.000000000000000 ) ;
#12346 = CARTESIAN_POINT ( 'NONE',  ( -17.77999999999999758, 0.000000000000000000, 0.000000000000000000 ) ) ;
#12347 = DIRECTION ( 'NONE',  ( 0.000000000000000000, -0.4539904997395540764, 0.8910065241883640130 ) ) ;
#12348 = ORIENTED_EDGE ( 'NONE', *, *, #9183, .T. ) ;
#12349 = CIRCLE ( 'NONE', #3542, 24.00000000002400569 ) ;
#12350 = ORIENTED_EDGE ( 'NONE', *, *, #648, .F. ) ;
#12351 = CARTESIAN_POINT ( 'NONE',  ( -12.50000000000000355, 0.000000000000000000, 0.000000000000000000 ) ) ;
#12352 = CYLINDRICAL_SURFACE ( 'NONE', #10194, 24.00000000002399858 ) ;
#12354 = CIRCLE ( 'NONE', #5965, 63.00000000006298961 ) ;
#12353 = DIRECTION ( 'NONE',  ( -1.000000000000000000, 0.000000000000000000, -0.000000000000000000 ) ) ;
#12355 = VERTEX_POINT ( 'NONE', #10028 ) ;
#12356 = DIRECTION ( 'NONE',  ( 0.9938152567191714803, 0.000000000000000000, -0.1110460963393456596 ) ) ;
#12357 = DIRECTION ( 'NONE',  ( 1.000000000000000000, 0.000000000000000000, 0.000000000000000000 ) ) ;
#12358 = DIRECTION ( 'NONE',  ( 0.000000000000000000, 0.000000000000000000, 1.000000000000000000 ) ) ;
#12359 = AXIS2_PLACEMENT_3D ( 'NONE', #408, #16220, #3171 ) ;
#12360 = ORIENTED_EDGE ( 'NONE', *, *, #5385, .F. ) ;
#12361 = FACE_OUTER_BOUND ( 'NONE', #4680, .T. ) ;
#12362 = VERTEX_POINT ( 'NONE', #6790 ) ;
#12363 = AXIS2_PLACEMENT_3D ( 'NONE', #13308, #16253, #13590 ) ;
#12364 = DIRECTION ( 'NONE',  ( -1.000000000000000000, -0.000000000000000000, -0.000000000000000000 ) ) ;
#12365 = VERTEX_POINT ( 'NONE', #4226 ) ;
#12366 = FACE_OUTER_BOUND ( 'NONE', #11287, .T. ) ;
#12367 = DIRECTION ( 'NONE',  ( -0.000000000000000000, 1.000000000000000000, 1.224646799147353207E-16 ) ) ;
#12368 = EDGE_CURVE ( 'NONE', #3956, #6304, #6540, .T. ) ;
#12369 = EDGE_CURVE ( 'NONE', #11663, #13852, #12796, .T. ) ;
#12370 = EDGE_CURVE ( 'NONE', #18064, #1091, #3207, .T. ) ;
#12371 = AXIS2_PLACEMENT_3D ( 'NONE', #5892, #8379, #11419 ) ;
#12372 = CIRCLE ( 'NONE', #8426, 12.00000000001200817 ) ;
#12373 = VECTOR ( 'NONE', #6082, 1000.000000000000000 ) ;
#12374 = ADVANCED_FACE ( 'NONE', ( #2789 ), #7158, .T. ) ;
#12375 = B_SPLINE_CURVE_WITH_KNOTS ( 'NONE', 3,
 ( #11263, #11449, #10024, #17086, #2786, #15641, #12590, #8587 ),
 .UNSPECIFIED., .F., .F.,
 ( 4, 2, 2, 4 ),
 ( 0.005725059856848645212, 0.006314084072593634418, 0.006903108288338624492, 0.008081156719828603771 ),
 .UNSPECIFIED. ) ;
#12376 = AXIS2_PLACEMENT_3D ( 'NONE', #18610, #18410, #4236 ) ;
#12377 = ORIENTED_EDGE ( 'NONE', *, *, #5976, .T. ) ;
#12378 = ORIENTED_EDGE ( 'NONE', *, *, #18029, .T. ) ;
#12379 = FACE_OUTER_BOUND ( 'NONE', #11113, .T. ) ;
#12380 = DIRECTION ( 'NONE',  ( 0.01644736842105263414, -0.9998647328874152862, 0.000000000000000000 ) ) ;
#12381 = DIRECTION ( 'NONE',  ( 0.000000000000000000, -0.8090169943749402348, -0.5877852522924830181 ) ) ;
#12382 = DIRECTION ( 'NONE',  ( 0.000000000000000000, 0.000000000000000000, 1.000000000000000000 ) ) ;
#12383 = EDGE_CURVE ( 'NONE', #12204, #11293, #14159, .T. ) ;
#12384 = CARTESIAN_POINT ( 'NONE',  ( 10.00000000000000000, -56.23315539212691050, 1.335003989221430487 ) ) ;
#12385 = AXIS2_PLACEMENT_3D ( 'NONE', #13141, #96, #8316 ) ;
#12386 = DIRECTION ( 'NONE',  ( 0.000000000000000000, 0.9510565162951543083, -0.3090169943749447867 ) ) ;
#12387 = ORIENTED_EDGE ( 'NONE', *, *, #5281, .T. ) ;
#12388 = CARTESIAN_POINT ( 'NONE',  ( -2.756197834950067094, -3.027510591568735254, -3.223146290109809797 ) ) ;
#12389 = AXIS2_PLACEMENT_3D ( 'NONE', #12265, #7607, #1800 ) ;
#12390 = LINE ( 'NONE', #18203, #2074 ) ;
#12391 = ORIENTED_EDGE ( 'NONE', *, *, #17963, .T. ) ;
#12392 = CIRCLE ( 'NONE', #6920, 27.29487558977753991 ) ;
#12393 = VECTOR ( 'NONE', #10328, 1000.000000000000000 ) ;
#12394 = EDGE_CURVE ( 'NONE', #728, #6735, #4316, .T. ) ;
#12395 = CONTEXT_DEPENDENT_SHAPE_REPRESENTATION ( #4879, #15164 ) ;
#12396 = VERTEX_POINT ( 'NONE', #11268 ) ;
#12397 = ORIENTED_EDGE ( 'NONE', *, *, #17845, .F. ) ;
#12398 = CIRCLE ( 'NONE', #6341, 12.00000000001200640 ) ;
#12399 = EDGE_CURVE ( 'NONE', #10145, #3496, #11431, .T. ) ;
#12400 = ORIENTED_EDGE ( 'NONE', *, *, #12161, .F. ) ;
#12401 = CIRCLE ( 'NONE', #12712, 24.00000000002399858 ) ;
#12402 = DIRECTION ( 'NONE',  ( 0.000000000000000000, -1.000000000000000000, 0.000000000000000000 ) ) ;
#12403 = DIRECTION ( 'NONE',  ( 0.000000000000000000, 0.000000000000000000, -1.000000000000000000 ) ) ;
#12404 = AXIS2_PLACEMENT_3D ( 'NONE', #15766, #1475, #7085 ) ;
#12405 = CIRCLE ( 'NONE', #10872, 24.00000000002399858 ) ;
#12406 = DIRECTION ( 'NONE',  ( -1.000000000000000000, 0.000000000000000000, 0.000000000000000000 ) ) ;
#12407 = SURFACE_STYLE_USAGE ( .BOTH. , #8226 ) ;
#12408 = DIRECTION ( 'NONE',  ( 0.000000000000000000, 0.000000000000000000, 1.000000000000000000 ) ) ;
#12409 = CARTESIAN_POINT ( 'NONE',  ( 5.000000000000000000, -22.76987570971544272, 23.88582760061473209 ) ) ;
#12410 = ORIENTED_EDGE ( 'NONE', *, *, #16856, .T. ) ;
#12411 = DIRECTION ( 'NONE',  ( 0.000000000000000000, 0.000000000000000000, 1.000000000000000000 ) ) ;
#12412 = ORIENTED_EDGE ( 'NONE', *, *, #4143, .F. ) ;
#12413 = DIRECTION ( 'NONE',  ( 0.03086419753086420623, -0.9995235871707959241, 0.000000000000000000 ) ) ;
#12414 = PLANE ( 'NONE',  #3885 ) ;
#12415 = AXIS2_PLACEMENT_3D ( 'NONE', #5192, #10992, #3769 ) ;
#12416 = ORIENTED_EDGE ( 'NONE', *, *, #8759, .F. ) ;
#12417 = ORIENTED_EDGE ( 'NONE', *, *, #5319, .T. ) ;
#12418 = CARTESIAN_POINT ( 'NONE',  ( -26.29305231718568336, -26.50000000000000000, -16.45302069950552237 ) ) ;
#12419 = DIRECTION ( 'NONE',  ( 6.123233995736766036E-17, -1.000000000000000000, 0.000000000000000000 ) ) ;
#12420 = CIRCLE ( 'NONE', #2372, 56.24900000005625600 ) ;
#12421 = CARTESIAN_POINT ( 'NONE',  ( -0.3461262719736137305, 4.658553426539289610, -3.671615880910373608 ) ) ;
#12422 = EDGE_LOOP ( 'NONE', ( #10730, #290, #3023 ) ) ;
#12423 = VECTOR ( 'NONE', #14400, 1000.000000000000000 ) ;
#12424 = AXIS2_PLACEMENT_3D ( 'NONE', #6578, #3921, #18376 ) ;
#12425 = B_SPLINE_CURVE_WITH_KNOTS ( 'NONE', 3,
 ( #251, #3391, #9188, #6056, #11866, #17678 ),
 .UNSPECIFIED., .F., .F.,
 ( 4, 2, 4 ),
 ( 0.002365888236227967761, 0.003551327329835077609, 0.004736766423442186590 ),
 .UNSPECIFIED. ) ;
#12426 = EDGE_CURVE ( 'NONE', #6304, #3956, #6254, .T. ) ;
#12427 = DIRECTION ( 'NONE',  ( -1.000000000000000000, 0.000000000000000000, 0.000000000000000000 ) ) ;
#12428 = CARTESIAN_POINT ( 'NONE',  ( 10.00000000000000000, -1.489278925039700052, 26.20671763660628173 ) ) ;
#12429 = AXIS2_PLACEMENT_3D ( 'NONE', #13941, #16600, #907 ) ;
#12430 = DIRECTION ( 'NONE',  ( 1.000000000000000000, -0.000000000000000000, -0.000000000000000000 ) ) ;
#12431 = VERTEX_POINT ( 'NONE', #5355 ) ;
#12432 = CARTESIAN_POINT ( 'NONE',  ( 10.00000000000000000, -18.64666490672410148, 53.06836994729227541 ) ) ;
#12433 = AXIS2_PLACEMENT_3D ( 'NONE', #8301, #5817, #20 ) ;
#12434 = VECTOR ( 'NONE', #2950, 1000.000000000000000 ) ;
#12435 = ORIENTED_EDGE ( 'NONE', *, *, #1280, .F. ) ;
#12436 = UNCERTAINTY_MEASURE_WITH_UNIT (LENGTH_MEASURE( 1.000000000000000082E-05 ), #5426, 'distance_accuracy_value', 'NONE');
#12437 = AXIS2_PLACEMENT_3D ( 'NONE', #6374, #459, #4653 ) ;
#12438 = DIRECTION ( 'NONE',  ( -1.000000000000000000, -0.000000000000000000, -0.000000000000000000 ) ) ;
#12439 = ORIENTED_EDGE ( 'NONE', *, *, #16807, .T. ) ;
#12440 = CYLINDRICAL_SURFACE ( 'NONE', #13278, 30.00000000000000000 ) ;
#12441 = LINE ( 'NONE', #9860, #17440 ) ;
#12442 = LINE ( 'NONE', #18249, #12170 ) ;
#12443 = ORIENTED_EDGE ( 'NONE', *, *, #15636, .T. ) ;
#12444 = ORIENTED_EDGE ( 'NONE', *, *, #11450, .F. ) ;
#12445 = CARTESIAN_POINT ( 'NONE',  ( 11.25000000000000000, 0.000000000000000000, 0.000000000000000000 ) ) ;
#12446 = EDGE_CURVE ( 'NONE', #3960, #15091, #16909, .T. ) ;
#12447 = VERTEX_POINT ( 'NONE', #2503 ) ;
#12448 = CARTESIAN_POINT ( 'NONE',  ( 0.000000000000000000, -30.00000000000000000, 20.00000000000000000 ) ) ;
#12449 = CIRCLE ( 'NONE', #2412, 63.00000000006298961 ) ;
#12450 = AXIS2_PLACEMENT_3D ( 'NONE', #4367, #4452, #6533 ) ;
#12451 = EDGE_CURVE ( 'NONE', #8692, #4390, #7465, .T. ) ;
#12452 = DIRECTION ( 'NONE',  ( 0.000000000000000000, 0.000000000000000000, 1.000000000000000000 ) ) ;
#12453 = DIRECTION ( 'NONE',  ( 0.000000000000000000, -1.000000000000000000, 0.000000000000000000 ) ) ;
#12454 = ORIENTED_EDGE ( 'NONE', *, *, #13315, .F. ) ;
#12455 = DIRECTION ( 'NONE',  ( -1.000000000000000000, 0.000000000000000000, 0.000000000000000000 ) ) ;
#12456 = CIRCLE ( 'NONE', #4856, 56.24900000005625600 ) ;
#12457 = EDGE_LOOP ( 'NONE', ( #17215, #11984, #12470, #7262 ) ) ;
#12458 = DIRECTION ( 'NONE',  ( -1.000000000000000000, -0.000000000000000000, -0.000000000000000000 ) ) ;
#12459 = CARTESIAN_POINT ( 'NONE',  ( 10.04305231718605285, -30.00000000000000000, -30.90933677959240811 ) ) ;
#12460 = FACE_OUTER_BOUND ( 'NONE', #785, .T. ) ;
#12461 = ORIENTED_EDGE ( 'NONE', *, *, #4455, .F. ) ;
#12462 = CARTESIAN_POINT ( 'NONE',  ( 0.000000000000000000, 0.000000000000000000, 0.000000000000000000 ) ) ;
#12463 = VERTEX_POINT ( 'NONE', #11358 ) ;
#12464 = CIRCLE ( 'NONE', #5472, 2.649999999999999467 ) ;
#12465 = CARTESIAN_POINT ( 'NONE',  ( 5.000000000000000000, -13.79392154159090467, -61.47135697633794393 ) ) ;
#12466 = DIRECTION ( 'NONE',  ( 0.000000000000000000, 0.000000000000000000, 1.000000000000000000 ) ) ;
#12467 = ORIENTED_EDGE ( 'NONE', *, *, #15884, .F. ) ;
#12468 = EDGE_LOOP ( 'NONE', ( #8497, #1282, #158 ) ) ;
#12469 = SURFACE_SIDE_STYLE ('',( #6661 ) ) ;
#12470 = ORIENTED_EDGE ( 'NONE', *, *, #9246, .F. ) ;
#12471 = DIRECTION ( 'NONE',  ( 0.000000000000000000, -1.000000000000000000, 0.000000000000000000 ) ) ;
#12472 = FACE_OUTER_BOUND ( 'NONE', #3728, .T. ) ;
#12473 = AXIS2_PLACEMENT_3D ( 'NONE', #4157, #13009, #8806 ) ;
#12474 = VECTOR ( 'NONE', #9472, 1000.000000000000000 ) ;
#12475 = ORIENTED_EDGE ( 'NONE', *, *, #15442, .T. ) ;
#12476 = EDGE_LOOP ( 'NONE', ( #403, #14777, #17371, #17114 ) ) ;
#12477 = DIRECTION ( 'NONE',  ( -1.000000000000000000, 0.000000000000000000, -0.000000000000000000 ) ) ;
#12478 = FACE_OUTER_BOUND ( 'NONE', #12307, .T. ) ;
#12479 = FACE_OUTER_BOUND ( 'NONE', #12036, .T. ) ;
#12480 = DIRECTION ( 'NONE',  ( -0.000000000000000000, 1.000000000000000000, -0.000000000000000000 ) ) ;
#12481 = EDGE_CURVE ( 'NONE', #4230, #7648, #13249, .T. ) ;
#12482 = EDGE_CURVE ( 'NONE', #15024, #12292, #14878, .T. ) ;
#12483 = DIRECTION ( 'NONE',  ( -1.000000000000000000, -0.000000000000000000, -0.000000000000000000 ) ) ;
#12484 = LINE ( 'NONE', #1912, #12332 ) ;
#12485 = ORIENTED_EDGE ( 'NONE', *, *, #6114, .F. ) ;
#12486 = CARTESIAN_POINT ( 'NONE',  ( -3.472371940586054251, -2.614027278893156669, -3.320322319202162031 ) ) ;
#12487 = CARTESIAN_POINT ( 'NONE',  ( 10.00000000000000000, -4.381479206522757686, -32.70783759231090215 ) ) ;
#12488 = EDGE_LOOP ( 'NONE', ( #10588, #11766, #13682, #18384 ) ) ;
#12489 = ITEM_DEFINED_TRANSFORMATION ( 'NONE', 'NONE', #15068,  #8017 ) ;
#12490 = EDGE_CURVE ( 'NONE', #9696, #2243, #8781, .T. ) ;
#12491 = ORIENTED_EDGE ( 'NONE', *, *, #10751, .T. ) ;
#12492 = VERTEX_POINT ( 'NONE', #1823 ) ;
#12493 = EDGE_CURVE ( 'NONE', #435, #1871, #5345, .T. ) ;
#12494 = EDGE_LOOP ( 'NONE', ( #547, #6655, #7028, #16121 ) ) ;
#12495 = CIRCLE ( 'NONE', #13417, 24.00000000002400569 ) ;
#12496 = DIRECTION ( 'NONE',  ( 0.000000000000000000, 0.4539904997395479147, -0.8910065241883673437 ) ) ;
#12497 = DIRECTION ( 'NONE',  ( 0.8191520442889875797, 0.000000000000000000, 0.5735764363510522656 ) ) ;
#12498 = DIRECTION ( 'NONE',  ( 0.000000000000000000, 0.000000000000000000, -1.000000000000000000 ) ) ;
#12499 = LINE ( 'NONE', #16417, #9011 ) ;
#12500 = EDGE_CURVE ( 'NONE', #8012, #168, #18726, .T. ) ;
#12501 = DIRECTION ( 'NONE',  ( 0.000000000000000000, 0.000000000000000000, 1.000000000000000000 ) ) ;
#12502 = EDGE_CURVE ( 'NONE', #1486, #6058, #7536, .T. ) ;
#12503 = CARTESIAN_POINT ( 'NONE',  ( 0.000000000000000000, -45.00825343885045271, 33.95787273855228960 ) ) ;
#12504 = CARTESIAN_POINT ( 'NONE',  ( 0.000000000000000000, 0.000000000000000000, 0.000000000000000000 ) ) ;
#12505 = DIRECTION ( 'NONE',  ( -1.000000000000000000, -0.000000000000000000, -0.000000000000000000 ) ) ;
#12506 = ORIENTED_EDGE ( 'NONE', *, *, #12481, .T. ) ;
#12507 = FACE_BOUND ( 'NONE', #9974, .T. ) ;
#12508 = EDGE_LOOP ( 'NONE', ( #4846, #7329, #2137, #15867 ) ) ;
#12509 = ADVANCED_FACE ( 'NONE', ( #2984 ), #479, .T. ) ;
#12510 = DIRECTION ( 'NONE',  ( 0.000000000000000000, 0.000000000000000000, -1.000000000000000000 ) ) ;
#12511 = DIRECTION ( 'NONE',  ( -0.000000000000000000, -1.000000000000000000, 0.000000000000000000 ) ) ;
#12512 = EDGE_LOOP ( 'NONE', ( #12803, #9361, #4824, #14059 ) ) ;
#12513 = VERTEX_POINT ( 'NONE', #16401 ) ;
#12514 = ADVANCED_FACE ( 'NONE', ( #11732 ), #309, .T. ) ;
#12515 = DIRECTION ( 'NONE',  ( -1.000000000000000000, -0.000000000000000000, -0.000000000000000000 ) ) ;
#12516 = AXIS2_PLACEMENT_3D ( 'NONE', #17957, #8040, #13683 ) ;
#12517 = DIRECTION ( 'NONE',  ( 6.123233995736766036E-17, -1.000000000000000000, 0.000000000000000000 ) ) ;
#12518 = CARTESIAN_POINT ( 'NONE',  ( 0.000000000000000000, 15.61693798565496394, 61.03368945066441142 ) ) ;
#12519 = ORIENTED_EDGE ( 'NONE', *, *, #16809, .F. ) ;
#12520 = TOROIDAL_SURFACE ( 'NONE', #5543, 2.700000000000000622, 0.2000000000000000111 ) ;
#12521 = CARTESIAN_POINT ( 'NONE',  ( 10.00000000000000000, 0.000000000000000000, 0.000000000000000000 ) ) ;
#12522 = LINE ( 'NONE', #5376, #1534 ) ;
#12523 = DIRECTION ( 'NONE',  ( 1.000000000000000000, 0.000000000000000000, 0.000000000000000000 ) ) ;
#12524 = DIRECTION ( 'NONE',  ( -0.000000000000000000, 1.000000000000000000, -0.000000000000000000 ) ) ;
#12525 = EDGE_LOOP ( 'NONE', ( #15693, #10594, #7201, #4446 ) ) ;
#12526 = CARTESIAN_POINT ( 'NONE',  ( 0.000000000000000000, -50.71018745830426866, -24.33982105418955655 ) ) ;
#12527 = EDGE_LOOP ( 'NONE', ( #8912, #13585 ) ) ;
#12528 = AXIS2_PLACEMENT_3D ( 'NONE', #11042, #3814, #14095 ) ;
#12529 = CARTESIAN_POINT ( 'NONE',  ( 0.000000000000000000, 18.64666490672370713, 53.06836994729239620 ) ) ;
#12530 = CYLINDRICAL_SURFACE ( 'NONE', #4947, 24.00000000002399503 ) ;
#12531 = DIRECTION ( 'NONE',  ( 1.000000000000000000, 0.000000000000000000, 0.000000000000000000 ) ) ;
#12532 = ORIENTED_EDGE ( 'NONE', *, *, #4122, .F. ) ;
#12533 = ORIENTED_EDGE ( 'NONE', *, *, #15287, .T. ) ;
#12534 = EDGE_CURVE ( 'NONE', #11963, #11942, #33, .T. ) ;
#12535 = CARTESIAN_POINT ( 'NONE',  ( 10.00000000000000000, -18.38754094778278869, 53.29895248911668659 ) ) ;
#12536 = PRESENTATION_STYLE_ASSIGNMENT (( #14152 ) ) ;
#12537 = ORIENTED_EDGE ( 'NONE', *, *, #17653, .F. ) ;
#12538 = DIRECTION ( 'NONE',  ( 0.000000000000000000, -0.5877852522924623679, -0.8090169943749552228 ) ) ;
#12539 = VECTOR ( 'NONE', #6047, 1000.000000000000000 ) ;
#12540 = VECTOR ( 'NONE', #15723, 1000.000000000000114 ) ;
#12541 = DIRECTION ( 'NONE',  ( 0.000000000000000000, 0.4999999999999990008, -0.8660254037844391517 ) ) ;
#12542 = AXIS2_PLACEMENT_3D ( 'NONE', #7900, #6471, #12763 ) ;
#12543 = DIRECTION ( 'NONE',  ( 0.000000000000000000, 1.000000000000000000, 0.000000000000000000 ) ) ;
#12544 = ORIENTED_EDGE ( 'NONE', *, *, #17170, .T. ) ;
#12545 = FACE_OUTER_BOUND ( 'NONE', #1936, .T. ) ;
#12546 = ORIENTED_EDGE ( 'NONE', *, *, #15279, .T. ) ;
#12547 = DIRECTION ( 'NONE',  ( 0.000000000000000000, 0.000000000000000000, 1.000000000000000000 ) ) ;
#12548 = DIRECTION ( 'NONE',  ( 1.000000000000000000, -0.000000000000000000, 0.000000000000000000 ) ) ;
#12549 = FACE_OUTER_BOUND ( 'NONE', #13247, .T. ) ;
#12550 = EDGE_LOOP ( 'NONE', ( #10777, #7529 ) ) ;
#12551 = CARTESIAN_POINT ( 'NONE',  ( 2.100000000000000089, 0.000000000000000000, -4.694516984716113228 ) ) ;
#12552 = ORIENTED_EDGE ( 'NONE', *, *, #13378, .T. ) ;
#12553 = CARTESIAN_POINT ( 'NONE',  ( 10.00000000000000000, -5.120903701083534543E-13, -45.00000000000000000 ) ) ;
#12554 = FACE_BOUND ( 'NONE', #10716, .T. ) ;
#12555 = ORIENTED_EDGE ( 'NONE', *, *, #5771, .F. ) ;
#12556 = ORIENTED_EDGE ( 'NONE', *, *, #2346, .F. ) ;
#12557 = EDGE_CURVE ( 'NONE', #14712, #9000, #16000, .T. ) ;
#12558 = CYLINDRICAL_SURFACE ( 'NONE', #17258, 12.00000000001200462 ) ;
#12559 = ORIENTED_EDGE ( 'NONE', *, *, #11860, .T. ) ;
#12560 = CARTESIAN_POINT ( 'NONE',  ( -56.50000000009000445, -30.00000000000000000, 3.817814120399276590E-13 ) ) ;
#12561 = VECTOR ( 'NONE', #13185, 1000.000000000000000 ) ;
#12562 = CARTESIAN_POINT ( 'NONE',  ( 10.00000000000000000, 1.489278925039520418, 26.20671763660628883 ) ) ;
#12563 = AXIS2_PLACEMENT_3D ( 'NONE', #14668, #5818, #17438 ) ;
#12564 = EDGE_CURVE ( 'NONE', #14282, #1187, #7259, .T. ) ;
#12565 = VERTEX_POINT ( 'NONE', #4498 ) ;
#12566 = AXIS2_PLACEMENT_3D ( 'NONE', #6813, #1208, #7007 ) ;
#12567 = VERTEX_POINT ( 'NONE', #10206 ) ;
#12568 = DIRECTION ( 'NONE',  ( 1.000000000000000000, 0.000000000000000000, 0.000000000000000000 ) ) ;
#12569 = CIRCLE ( 'NONE', #11954, 25.00000000000000000 ) ;
#12570 = DIRECTION ( 'NONE',  ( 1.000000000000000000, 0.000000000000000000, -0.000000000000000000 ) ) ;
#12571 = CYLINDRICAL_SURFACE ( 'NONE', #1142, 63.00000000006298961 ) ;
#12572 = DIRECTION ( 'NONE',  ( -0.000000000000000000, 1.000000000000000000, -0.000000000000000000 ) ) ;
#12573 = EDGE_CURVE ( 'NONE', #18077, #9531, #11728, .T. ) ;
#12574 = CARTESIAN_POINT ( 'NONE',  ( 0.000000000000000000, -53.22058882792172341, -33.71303790549333712 ) ) ;
#12575 = CARTESIAN_POINT ( 'NONE',  ( -10.00000000000000000, 0.000000000000000000, 0.000000000000000000 ) ) ;
#12576 = DIRECTION ( 'NONE',  ( 0.000000000000000000, 0.5000000000000009992, 0.8660254037844380415 ) ) ;
#12577 = ORIENTED_EDGE ( 'NONE', *, *, #1376, .F. ) ;
#12578 = PLANE ( 'NONE',  #13077 ) ;
#12579 = CARTESIAN_POINT ( 'NONE',  ( 5.000000000000000000, -62.72529079327811274, 5.876895005582225551 ) ) ;
#12580 = CARTESIAN_POINT ( 'NONE',  ( 0.000000000000000000, 6.681932690257323060, -25.38428207620315291 ) ) ;
#12581 = ORIENTED_EDGE ( 'NONE', *, *, #10018, .F. ) ;
#12582 = VECTOR ( 'NONE', #4611, 1000.000000000000000 ) ;
#12583 = EDGE_LOOP ( 'NONE', ( #13996, #8638, #14662, #17573 ) ) ;
#12584 = EDGE_CURVE ( 'NONE', #6251, #12565, #4731, .T. ) ;
#12585 = ORIENTED_EDGE ( 'NONE', *, *, #14641, .T. ) ;
#12586 = EDGE_LOOP ( 'NONE', ( #11464, #16090, #12851, #10348 ) ) ;
#12587 = CARTESIAN_POINT ( 'NONE',  ( 10.00000000000000000, 10.11537145609457156, -55.33199130079773909 ) ) ;
#12588 = CARTESIAN_POINT ( 'NONE',  ( -117.1020693116508085, -34.99999999999999289, 17.04080595179778967 ) ) ;
#12589 = CARTESIAN_POINT ( 'NONE',  ( 10.00000000000000000, 24.33982105418901298, 50.71018745830453156 ) ) ;
#12590 = CARTESIAN_POINT ( 'NONE',  ( 3.999999999999999112, 1.941961291383486277, -0.3515519931180248192 ) ) ;
#12591 = CARTESIAN_POINT ( 'NONE',  ( -5.384454397937118664, 6.702023979852544604E-16, -5.000000000000000000 ) ) ;
#12592 = DIRECTION ( 'NONE',  ( -1.000000000000000000, 0.000000000000000000, 0.000000000000000000 ) ) ;
#12593 = DIRECTION ( 'NONE',  ( -0.000000000000000000, 1.000000000000000000, -0.000000000000000000 ) ) ;
#12594 = DIRECTION ( 'NONE',  ( 0.000000000000000000, 1.000000000000000000, 0.000000000000000000 ) ) ;
#12595 = ORIENTED_EDGE ( 'NONE', *, *, #13415, .T. ) ;
#12596 = DIRECTION ( 'NONE',  ( 0.000000000000000000, 0.000000000000000000, 1.000000000000000000 ) ) ;
#12597 = EDGE_LOOP ( 'NONE', ( #10881, #18548, #2081, #7763 ) ) ;
#12598 = CYLINDRICAL_SURFACE ( 'NONE', #2548, 2.500000000000000444 ) ;
#12599 = CARTESIAN_POINT ( 'NONE',  ( -10.00000000000000000, 0.000000000000000000, 0.000000000000000000 ) ) ;
#12600 = ORIENTED_EDGE ( 'NONE', *, *, #5533, .F. ) ;
#12601 = ORIENTED_EDGE ( 'NONE', *, *, #14169, .F. ) ;
#12602 = LINE ( 'NONE', #12418, #17530 ) ;
#12603 = DIRECTION ( 'NONE',  ( 0.3090169943749448422, 6.123233995736766036E-17, 0.9510565162951546414 ) ) ;
#12604 = CARTESIAN_POINT ( 'NONE',  ( 2.500000000000000000, -2.357898499370431722, 2.818925648462311528E-15 ) ) ;
#12605 = ORIENTED_EDGE ( 'NONE', *, *, #10832, .T. ) ;
#12606 = EDGE_CURVE ( 'NONE', #9916, #3285, #7167, .T. ) ;
#12607 = EDGE_CURVE ( 'NONE', #10536, #1171, #5025, .T. ) ;
#12608 = EDGE_CURVE ( 'NONE', #16951, #8709, #16020, .T. ) ;
#12609 = ADVANCED_BREP_SHAPE_REPRESENTATION ( '', ( #15813, #8017 ), #16855 ) ;
#12610 = CARTESIAN_POINT ( 'NONE',  ( 10.00000000000000000, 53.92768374110868734, 16.45250512421953459 ) ) ;
#12611 = EDGE_CURVE ( 'NONE', #15930, #8606, #5940, .T. ) ;
#12612 = DIRECTION ( 'NONE',  ( 0.000000000000000000, -1.000000000000000000, 0.000000000000000000 ) ) ;
#12613 = DIRECTION ( 'NONE',  ( 0.000000000000000000, 0.000000000000000000, -1.000000000000000000 ) ) ;
#12614 = DIRECTION ( 'NONE',  ( 0.000000000000000000, 0.000000000000000000, -1.000000000000000000 ) ) ;
#12615 = EDGE_CURVE ( 'NONE', #353, #10104, #14679, .T. ) ;
#12616 = EDGE_CURVE ( 'NONE', #7427, #10448, #13570, .T. ) ;
#12617 = UNCERTAINTY_MEASURE_WITH_UNIT (LENGTH_MEASURE( 1.000000000000000082E-05 ), #4491, 'distance_accuracy_value', 'NONE');
#12618 = DIRECTION ( 'NONE',  ( -1.000000000000000000, -0.000000000000000000, -0.000000000000000000 ) ) ;
#12619 = ORIENTED_EDGE ( 'NONE', *, *, #14834, .T. ) ;
#12620 = EDGE_CURVE ( 'NONE', #3492, #2015, #12484, .T. ) ;
#12621 = DIRECTION ( 'NONE',  ( -1.000000000000000000, -0.000000000000000000, -0.000000000000000000 ) ) ;
#12622 = FACE_OUTER_BOUND ( 'NONE', #6503, .T. ) ;
#12623 = DIRECTION ( 'NONE',  ( 0.000000000000000000, -0.9876883405951394357, 0.1564344650402205994 ) ) ;
#12624 = ORIENTED_EDGE ( 'NONE', *, *, #8610, .T. ) ;
#12625 = AXIS2_PLACEMENT_3D ( 'NONE', #17988, #10740, #3511 ) ;
#12626 = VERTEX_POINT ( 'NONE', #2283 ) ;
#12627 = AXIS2_PLACEMENT_3D ( 'NONE', #10648, #8745, #13226 ) ;
#12628 = CYLINDRICAL_SURFACE ( 'NONE', #474, 24.00000000002400213 ) ;
#12629 =( LENGTH_UNIT ( ) NAMED_UNIT ( * ) SI_UNIT ( .MILLI., .METRE. ) );
#12630 = ORIENTED_EDGE ( 'NONE', *, *, #13674, .T. ) ;
#12631 = DIRECTION ( 'NONE',  ( 0.000000000000000000, -1.000000000000000000, 0.000000000000000000 ) ) ;
#12632 = EDGE_CURVE ( 'NONE', #186, #16875, #15684, .T. ) ;
#12633 = AXIS2_PLACEMENT_3D ( 'NONE', #18233, #5181, #13948 ) ;
#12634 = LINE ( 'NONE', #2347, #1970 ) ;
#12635 = AXIS2_PLACEMENT_3D ( 'NONE', #9275, #429, #246 ) ;
#12637 = AXIS2_PLACEMENT_3D ( 'NONE', #12304, #16708, #3658 ) ;
#12636 = CARTESIAN_POINT ( 'NONE',  ( 10.00000000000000000, -24.46385708179976604, -9.514709542737152859 ) ) ;
#12638 = EDGE_CURVE ( 'NONE', #8411, #13451, #13811, .T. ) ;
#12639 = VERTEX_POINT ( 'NONE', #3445 ) ;
#12640 = CARTESIAN_POINT ( 'NONE',  ( -3.333333333333332149, -2.694301256218264218, -3.300726591567082036 ) ) ;
#12641 = VERTEX_POINT ( 'NONE', #14969 ) ;
#12642 = CARTESIAN_POINT ( 'NONE',  ( -87.76214430591549842, -10.00000000000001954, 4.471241649927994999 ) ) ;
#12643 = DIRECTION ( 'NONE',  ( 0.000000000000000000, 0.000000000000000000, 1.000000000000000000 ) ) ;
#12644 = CYLINDRICAL_SURFACE ( 'NONE', #1468, 12.00000000001200462 ) ;
#12645 = ORIENTED_EDGE ( 'NONE', *, *, #9564, .F. ) ;
#12646 = DIRECTION ( 'NONE',  ( 1.000000000000000000, 0.000000000000000000, 0.000000000000000000 ) ) ;
#12647 = ORIENTED_EDGE ( 'NONE', *, *, #2447, .F. ) ;
#12648 = LINE ( 'NONE', #8180, #9685 ) ;
#12649 = CARTESIAN_POINT ( 'NONE',  ( 0.000000000000000000, -4.007856633822952652, -62.87238730325625369 ) ) ;
#12650 = VECTOR ( 'NONE', #2340, 1000.000000000000000 ) ;
#12651 = ORIENTED_EDGE ( 'NONE', *, *, #3480, .F. ) ;
#12652 = VERTEX_POINT ( 'NONE', #6391 ) ;
#12653 = AXIS2_PLACEMENT_3D ( 'NONE', #2527, #2721, #11289 ) ;
#12654 = DIRECTION ( 'NONE',  ( -1.000000000000000000, 0.000000000000000000, -0.000000000000000000 ) ) ;
#12655 = ORIENTED_EDGE ( 'NONE', *, *, #1925, .T. ) ;
#12656 = ORIENTED_EDGE ( 'NONE', *, *, #16442, .T. ) ;
#12657 = CARTESIAN_POINT ( 'NONE',  ( 3.061616997868383043E-15, 13.24999999999999822, -25.00000000000000000 ) ) ;
#12658 = DIRECTION ( 'NONE',  ( -0.000000000000000000, -1.000000000000000000, -0.000000000000000000 ) ) ;
#12659 = CIRCLE ( 'NONE', #11130, 24.00000000002399858 ) ;
#12660 = CIRCLE ( 'NONE', #18133, 56.24900000005625600 ) ;
#12661 = CIRCLE ( 'NONE', #16312, 63.00000000006298961 ) ;
#12662 = ADVANCED_FACE ( 'NONE', ( #10949 ), #6483, .T. ) ;
#12663 = ORIENTED_EDGE ( 'NONE', *, *, #1771, .F. ) ;
#12664 = TOROIDAL_SURFACE ( 'NONE', #13273, 4.000000000000000000, 0.2500000000000000000 ) ;
#12665 = VECTOR ( 'NONE', #18778, 1000.000000000000114 ) ;
#12666 = ORIENTED_EDGE ( 'NONE', *, *, #18788, .F. ) ;
#12667 = DIRECTION ( 'NONE',  ( -1.000000000000000000, 0.000000000000000000, -0.000000000000000000 ) ) ;
#12668 = CARTESIAN_POINT ( 'NONE',  ( -6.473970235329672780E-16, -4.862606272033106691, -3.745885042887442395 ) ) ;
#12669 = DIRECTION ( 'NONE',  ( -0.000000000000000000, 1.000000000000000000, -0.000000000000000000 ) ) ;
#12670 = DIRECTION ( 'NONE',  ( 0.000000000000000000, 0.1564344650402244297, 0.9876883405951387696 ) ) ;
#12671 = DIRECTION ( 'NONE',  ( -0.000000000000000000, 1.000000000000000000, -0.000000000000000000 ) ) ;
#12672 = DIRECTION ( 'NONE',  ( -1.000000000000000000, 0.000000000000000000, 0.000000000000000000 ) ) ;
#12673 = DIRECTION ( 'NONE',  ( 1.000000000000000000, -0.000000000000000000, 0.000000000000000000 ) ) ;
#12674 = VERTEX_POINT ( 'NONE', #11043 ) ;
#12675 = DIRECTION ( 'NONE',  ( -1.000000000000000000, 0.000000000000000000, -0.000000000000000000 ) ) ;
#12676 =( REPRESENTATION_RELATIONSHIP ('NONE','NONE', #11014, #16765 ) REPRESENTATION_RELATIONSHIP_WITH_TRANSFORMATION ( #9628 )SHAPE_REPRESENTATION_RELATIONSHIP( ) );
#12677 = DIRECTION ( 'NONE',  ( 0.000000000000000000, 0.000000000000000000, 1.000000000000000000 ) ) ;
#12678 = FACE_BOUND ( 'NONE', #16557, .T. ) ;
#12679 = DIRECTION ( 'NONE',  ( 0.000000000000000000, -0.8910065241883626808, -0.4539904997395571296 ) ) ;
#12680 = CIRCLE ( 'NONE', #13290, 24.00000000002399858 ) ;
#12681 = AXIS2_PLACEMENT_3D ( 'NONE', #14284, #8467, #7214 ) ;
#12682 = ITEM_DEFINED_TRANSFORMATION ( 'NONE', 'NONE', #466,  #8017 ) ;
#12683 = AXIS2_PLACEMENT_3D ( 'NONE', #2104, #7909, #9809 ) ;
#12684 = VERTEX_POINT ( 'NONE', #10850 ) ;
#12685 = AXIS2_PLACEMENT_3D ( 'NONE', #7882, #7425, #10300 ) ;
#12686 = AXIS2_PLACEMENT_3D ( 'NONE', #15435, #8201, #4951 ) ;
#12687 = EDGE_CURVE ( 'NONE', #7169, #17591, #2295, .T. ) ;
#12688 = VERTEX_POINT ( 'NONE', #8102 ) ;
#12689 = ORIENTED_EDGE ( 'NONE', *, *, #12014, .F. ) ;
#12690 = DIRECTION ( 'NONE',  ( -1.000000000000000000, -0.000000000000000000, 0.000000000000000000 ) ) ;
#12691 = VECTOR ( 'NONE', #15134, 1000.000000000000000 ) ;
#12692 = CARTESIAN_POINT ( 'NONE',  ( 0.000000000000000000, 10.00000000000000000, 0.000000000000000000 ) ) ;
#12693 = DIRECTION ( 'NONE',  ( 0.000000000000000000, 0.000000000000000000, 1.000000000000000000 ) ) ;
#12695 = CARTESIAN_POINT ( 'NONE',  ( 3.678949249685231848, 0.000000000000000000, 0.000000000000000000 ) ) ;
#12694 = AXIS2_PLACEMENT_3D ( 'NONE', #11, #5807, #16182 ) ;
#12696 = DIRECTION ( 'NONE',  ( 0.000000000000000000, 0.000000000000000000, 1.000000000000000000 ) ) ;
#12697 = CARTESIAN_POINT ( 'NONE',  ( 11.25000000000000000, 0.000000000000000000, 0.000000000000000000 ) ) ;
#12698 = AXIS2_PLACEMENT_3D ( 'NONE', #7861, #12232, #17761 ) ;
#12699 = CARTESIAN_POINT ( 'NONE',  ( -11.15000000000000391, 0.000000000000000000, 0.000000000000000000 ) ) ;
#12700 = EDGE_LOOP ( 'NONE', ( #5975, #16067, #468, #9152 ) ) ;
#12701 = AXIS2_PLACEMENT_3D ( 'NONE', #9166, #16705, #3561 ) ;
#12702 = DIRECTION ( 'NONE',  ( 0.000000000000000000, 1.000000000000000000, 3.469446951950143595E-15 ) ) ;
#12703 = EDGE_LOOP ( 'NONE', ( #10865, #936, #18625, #12337 ) ) ;
#12704 = CARTESIAN_POINT ( 'NONE',  ( 0.000000000000000000, 0.000000000000000000, 0.000000000000000000 ) ) ;
#12705 = FACE_BOUND ( 'NONE', #5209, .T. ) ;
#12706 = ORIENTED_EDGE ( 'NONE', *, *, #16565, .F. ) ;
#12707 = DIRECTION ( 'NONE',  ( 0.000000000000000000, 0.000000000000000000, -1.000000000000000000 ) ) ;
#12708 = DIRECTION ( 'NONE',  ( 0.4827112169034774025, 7.285838599102588564E-17, 0.8757795847560982949 ) ) ;
#12709 = DIRECTION ( 'NONE',  ( 0.000000000000000000, 1.000000000000000000, 0.000000000000000000 ) ) ;
#12710 = VERTEX_POINT ( 'NONE', #3727 ) ;
#12711 = AXIS2_PLACEMENT_3D ( 'NONE', #11112, #11308, #8358 ) ;
#12712 = AXIS2_PLACEMENT_3D ( 'NONE', #6886, #2314, #2509 ) ;
#12713 = CIRCLE ( 'NONE', #8763, 29.90000000000000213 ) ;
#12714 = CARTESIAN_POINT ( 'NONE',  ( 0.000000000000000000, 0.000000000000000000, 0.000000000000000000 ) ) ;
#12715 = CYLINDRICAL_SURFACE ( 'NONE', #14307, 2.649999999999992806 ) ;
#12716 = FACE_OUTER_BOUND ( 'NONE', #2459, .T. ) ;
#12717 = CARTESIAN_POINT ( 'NONE',  ( -12.50000000000000533, 0.000000000000000000, 0.000000000000000000 ) ) ;
#12718 = AXIS2_PLACEMENT_3D ( 'NONE', #11482, #7089, #17382 ) ;
#12719 = DIRECTION ( 'NONE',  ( 1.000000000000000000, 0.000000000000000000, 0.000000000000000000 ) ) ;
#12720 = VERTEX_POINT ( 'NONE', #483 ) ;
#12721 = EDGE_CURVE ( 'NONE', #15712, #2367, #9297, .T. ) ;
#12722 = EDGE_CURVE ( 'NONE', #9305, #16545, #3637, .T. ) ;
#12723 = DIRECTION ( 'NONE',  ( -0.000000000000000000, -0.000000000000000000, 1.000000000000000000 ) ) ;
#12724 = FACE_OUTER_BOUND ( 'NONE', #11067, .T. ) ;
#12725 = DIRECTION ( 'NONE',  ( -1.000000000000000000, 0.000000000000000000, 0.000000000000000000 ) ) ;
#12726 = CIRCLE ( 'NONE', #2065, 12.00000000001200640 ) ;
#12727 = ORIENTED_EDGE ( 'NONE', *, *, #18358, .T. ) ;
#12728 = ORIENTED_EDGE ( 'NONE', *, *, #4811, .F. ) ;
#12729 = VECTOR ( 'NONE', #8101, 1000.000000000000114 ) ;
#12730 = FACE_BOUND ( 'NONE', #13594, .T. ) ;
#12731 = PRESENTATION_STYLE_ASSIGNMENT (( #11096 ) ) ;
#12732 = EDGE_CURVE ( 'NONE', #14348, #15928, #9432, .T. ) ;
#12733 = ORIENTED_EDGE ( 'NONE', *, *, #11900, .T. ) ;
#12734 = CARTESIAN_POINT ( 'NONE',  ( 10.00000000000000000, 12.18267823974788122, -25.42247726998001411 ) ) ;
#12735 = EDGE_CURVE ( 'NONE', #9197, #1805, #6579, .T. ) ;
#12736 = AXIS2_PLACEMENT_3D ( 'NONE', #5748, #14119, #8322 ) ;
#12737 = VECTOR ( 'NONE', #10836, 1000.000000000000000 ) ;
#12738 = CARTESIAN_POINT ( 'NONE',  ( 5.000000000000000000, 4.007856633823394077, 62.87238730325622527 ) ) ;
#12739 = EDGE_CURVE ( 'NONE', #7605, #16334, #4142, .T. ) ;
#12740 = VECTOR ( 'NONE', #11020, 1000.000000000000114 ) ;
#12741 = DIRECTION ( 'NONE',  ( -1.000000000000000000, 0.000000000000000000, 0.000000000000000000 ) ) ;
#12742 = ORIENTED_EDGE ( 'NONE', *, *, #3172, .F. ) ;
#12743 = DIRECTION ( 'NONE',  ( 0.8191520442889902442, 1.003171929053522651E-16, -0.5735764363510482688 ) ) ;
#12744 = ORIENTED_EDGE ( 'NONE', *, *, #15810, .T. ) ;
#12745 = DIRECTION ( 'NONE',  ( 0.000000000000000000, 0.000000000000000000, 1.000000000000000000 ) ) ;
#12746 = CARTESIAN_POINT ( 'NONE',  ( -79.64793068852898728, -38.00000000000000000, -31.86039329588756530 ) ) ;
#12747 = LINE ( 'NONE', #5120, #9664 ) ;
#12748 = ORIENTED_EDGE ( 'NONE', *, *, #5431, .T. ) ;
#12749 = FACE_OUTER_BOUND ( 'NONE', #310, .T. ) ;
#12751 = ORIENTED_EDGE ( 'NONE', *, *, #18201, .T. ) ;
#12750 = EDGE_CURVE ( 'NONE', #5171, #14997, #12959, .T. ) ;
#12752 = EDGE_CURVE ( 'NONE', #14440, #5933, #4866, .T. ) ;
#12753 = DIRECTION ( 'NONE',  ( -1.000000000000000000, 0.000000000000000000, 0.000000000000000000 ) ) ;
#12754 = DIRECTION ( 'NONE',  ( -1.000000000000000000, -0.000000000000000000, 0.000000000000000000 ) ) ;
#12755 = CIRCLE ( 'NONE', #5466, 63.00000000006298961 ) ;
#12756 = ORIENTED_EDGE ( 'NONE', *, *, #2827, .F. ) ;
#12757 = ORIENTED_EDGE ( 'NONE', *, *, #8259, .T. ) ;
#12758 = CARTESIAN_POINT ( 'NONE',  ( 10.00000000000000000, -7.813799127872885997, -55.83748330407415494 ) ) ;
#12759 = CIRCLE ( 'NONE', #18227, 29.90000000000000213 ) ;
#12760 = EDGE_CURVE ( 'NONE', #2267, #16127, #15334, .T. ) ;
#12761 = ORIENTED_EDGE ( 'NONE', *, *, #18797, .F. ) ;
#12762 = LINE ( 'NONE', #11409, #1491 ) ;
#12763 = DIRECTION ( 'NONE',  ( 0.000000000000000000, 0.9876883405951371042, 0.1564344650402347547 ) ) ;
#12764 = EDGE_CURVE ( 'NONE', #858, #16875, #16291, .T. ) ;
#12765 = CIRCLE ( 'NONE', #7901, 56.24900000005626310 ) ;
#12766 = ORIENTED_EDGE ( 'NONE', *, *, #3, .T. ) ;
#12767 = VECTOR ( 'NONE', #5109, 1000.000000000000000 ) ;
#12768 = VERTEX_POINT ( 'NONE', #18004 ) ;
#12769 = CARTESIAN_POINT ( 'NONE',  ( 10.00000000000000000, -16.45250512421816680, -53.92768374110909235 ) ) ;
#12770 = LINE ( 'NONE', #5613, #12434 ) ;
#12771 = DIRECTION ( 'NONE',  ( -1.000000000000000000, -0.000000000000000000, 0.000000000000000000 ) ) ;
#12772 = CARTESIAN_POINT ( 'NONE',  ( -26.29305231718568336, -26.50000000000000000, -19.10302069950552095 ) ) ;
#12773 = CARTESIAN_POINT ( 'NONE',  ( 0.000000000000000000, -4.007856633823831061, 62.87238730325619684 ) ) ;
#12774 = DIRECTION ( 'NONE',  ( 0.000000000000000000, 0.000000000000000000, 1.000000000000000000 ) ) ;
#12775 = DIRECTION ( 'NONE',  ( -0.000000000000000000, 1.000000000000000000, -0.000000000000000000 ) ) ;
#12776 = ORIENTED_EDGE ( 'NONE', *, *, #12534, .F. ) ;
#12777 = CARTESIAN_POINT ( 'NONE',  ( 2.500000000000000000, 2.357898499370431722, -2.818925648462311528E-15 ) ) ;
#12778 = CARTESIAN_POINT ( 'NONE',  ( 10.00000000000000000, 0.000000000000000000, 0.000000000000000000 ) ) ;
#12779 = DIRECTION ( 'NONE',  ( -1.000000000000000000, 0.000000000000000000, 0.000000000000000000 ) ) ;
#12780 = CIRCLE ( 'NONE', #4552, 63.00000000006298961 ) ;
#12781 = CYLINDRICAL_SURFACE ( 'NONE', #14386, 12.00000000001200462 ) ;
#12782 = EDGE_CURVE ( 'NONE', #1018, #5360, #4954, .T. ) ;
#12783 = AXIS2_PLACEMENT_3D ( 'NONE', #11184, #4246, #8244 ) ;
#12784 = ORIENTED_EDGE ( 'NONE', *, *, #4160, .F. ) ;
#12785 = ORIENTED_EDGE ( 'NONE', *, *, #7087, .F. ) ;
#12786 = LINE ( 'NONE', #11352, #16956 ) ;
#12787 =( NAMED_UNIT ( * ) SI_UNIT ( $, .STERADIAN. ) SOLID_ANGLE_UNIT ( ) );
#12788 = VERTEX_POINT ( 'NONE', #3534 ) ;
#12789 = AXIS2_PLACEMENT_3D ( 'NONE', #2614, #8433, #14243 ) ;
#12790 = DIRECTION ( 'NONE',  ( 0.000000000000000000, 0.000000000000000000, 1.000000000000000000 ) ) ;
#12791 = APPLICATION_CONTEXT ( 'automotive_design' ) ;
#12792 = DIRECTION ( 'NONE',  ( 0.000000000000000000, 0.000000000000000000, 1.000000000000000000 ) ) ;
#12793 = EDGE_CURVE ( 'NONE', #11392, #192, #18747, .T. ) ;
#12794 = DIRECTION ( 'NONE',  ( -1.000000000000000000, 0.000000000000000000, -0.000000000000000000 ) ) ;
#12795 = LINE ( 'NONE', #18598, #4616 ) ;
#12796 = LINE ( 'NONE', #5746, #11414 ) ;
#12797 = VERTEX_POINT ( 'NONE', #7911 ) ;
#12798 = DIRECTION ( 'NONE',  ( -1.000000000000000000, -0.000000000000000000, -0.000000000000000000 ) ) ;
#12799 = ORIENTED_EDGE ( 'NONE', *, *, #6193, .T. ) ;
#12800 = EDGE_CURVE ( 'NONE', #2367, #15712, #14434, .T. ) ;
#12801 = CARTESIAN_POINT ( 'NONE',  ( 0.000000000000000000, 0.000000000000000000, 0.000000000000000000 ) ) ;
#12802 = CARTESIAN_POINT ( 'NONE',  ( 11.14999999999999680, 0.000000000000000000, 29.90000000000000213 ) ) ;
#12803 = ORIENTED_EDGE ( 'NONE', *, *, #291, .T. ) ;
#12804 = FACE_OUTER_BOUND ( 'NONE', #11044, .T. ) ;
#12805 = DIRECTION ( 'NONE',  ( 6.123233995736766036E-17, -1.000000000000000000, 0.000000000000000000 ) ) ;
#12806 = CARTESIAN_POINT ( 'NONE',  ( 0.2500000000000002220, 5.204748896376250699E-16, -4.250000000000000000 ) ) ;
#12807 = ORIENTED_EDGE ( 'NONE', *, *, #2608, .F. ) ;
#12808 = EDGE_CURVE ( 'NONE', #7462, #17978, #7180, .T. ) ;
#12809 = VECTOR ( 'NONE', #12743, 1000.000000000000114 ) ;
#12810 = DIRECTION ( 'NONE',  ( 0.000000000000000000, -0.000000000000000000, 1.000000000000000000 ) ) ;
#12811 = CARTESIAN_POINT ( 'NONE',  ( 10.00000000000000000, 53.06836994729233936, 18.64666490672390964 ) ) ;
#12812 = DIRECTION ( 'NONE',  ( -1.000000000000000000, -0.000000000000000000, -0.000000000000000000 ) ) ;
#12813 = EDGE_CURVE ( 'NONE', #8705, #12674, #9724, .T. ) ;
#12814 = DIRECTION ( 'NONE',  ( -1.000000000000000000, -0.000000000000000000, -0.000000000000000000 ) ) ;
#12815 = ADVANCED_FACE ( 'NONE', ( #14008 ), #3816, .T. ) ;
#12816 = DIRECTION ( 'NONE',  ( -0.000000000000000000, -0.000000000000000000, 1.000000000000000000 ) ) ;
#12817 = ORIENTED_EDGE ( 'NONE', *, *, #17629, .T. ) ;
#12818 = CIRCLE ( 'NONE', #17384, 24.00000000002399503 ) ;
#12819 = ADVANCED_FACE ( 'NONE', ( #11428 ), #5446, .F. ) ;
#12820 = CARTESIAN_POINT ( 'NONE',  ( 0.000000000000000000, -26.71881558261766898, 49.49802920186213129 ) ) ;
#12821 = DIRECTION ( 'NONE',  ( 0.000000000000000000, 0.000000000000000000, -1.000000000000000000 ) ) ;
#12822 = CYLINDRICAL_SURFACE ( 'NONE', #1821, 33.00000000003299760 ) ;
#12823 = EDGE_LOOP ( 'NONE', ( #12336, #14118, #9757, #1153 ) ) ;
#12824 = VERTEX_POINT ( 'NONE', #5721 ) ;
#12825 = FACE_BOUND ( 'NONE', #9621, .T. ) ;
#12826 = ORIENTED_EDGE ( 'NONE', *, *, #3804, .T. ) ;
#12827 = CARTESIAN_POINT ( 'NONE',  ( 0.000000000000000000, 57.83923611457320391, 24.97244012287522352 ) ) ;
#12828 = EDGE_CURVE ( 'NONE', #7635, #9528, #17824, .T. ) ;
#12829 = AXIS2_PLACEMENT_3D ( 'NONE', #1292, #6124, #6213 ) ;
#12830 = CYLINDRICAL_SURFACE ( 'NONE', #12955, 63.00000000006298961 ) ;
#12831 = EDGE_CURVE ( 'NONE', #15594, #4230, #8572, .T. ) ;
#12832 = DIRECTION ( 'NONE',  ( -1.000000000000000000, 0.000000000000000000, -0.000000000000000000 ) ) ;
#12833 = ORIENTED_EDGE ( 'NONE', *, *, #13325, .T. ) ;
#12834 = PLANE ( 'NONE',  #13717 ) ;
#12835 = AXIS2_PLACEMENT_3D ( 'NONE', #4457, #8923, #17419 ) ;
#12836 = ADVANCED_FACE ( 'NONE', ( #17251 ), #1161, .T. ) ;
#12837 = ORIENTED_EDGE ( 'NONE', *, *, #7937, .F. ) ;
#12839 = CARTESIAN_POINT ( 'NONE',  ( -1.655952806101422814, 3.662737355149034979, -7.623296525288699970E-18 ) ) ;
#12838 = PRODUCT_DEFINITION_CONTEXT ( 'detailed design', #2206, 'design' ) ;
#12840 = CARTESIAN_POINT ( 'NONE',  ( 2.000000000000000000, -6.429618962271402616, -1.000000000000000000 ) ) ;
#12841 = CARTESIAN_POINT ( 'NONE',  ( 0.000000000000000000, 53.89344778774834310, -16.10733642026427148 ) ) ;
#12842 = ORIENTED_EDGE ( 'NONE', *, *, #10391, .T. ) ;
#12843 = CARTESIAN_POINT ( 'NONE',  ( 1.836970198721030062E-14, 10.00000000000000000, 150.0000000000000284 ) ) ;
#12844 = ORIENTED_EDGE ( 'NONE', *, *, #1568, .F. ) ;
#12845 = FACE_OUTER_BOUND ( 'NONE', #2322, .T. ) ;
#12846 = DIRECTION ( 'NONE',  ( 1.000000000000000000, 0.000000000000000000, 0.000000000000000000 ) ) ;
#12847 = ORIENTED_EDGE ( 'NONE', *, *, #476, .F. ) ;
#12848 = ORIENTED_EDGE ( 'NONE', *, *, #6751, .T. ) ;
#12849 = DIRECTION ( 'NONE',  ( 0.000000000000000000, 1.000000000000000000, 0.000000000000000000 ) ) ;
#12850 = FILL_AREA_STYLE ('',( #5046 ) ) ;
#12852 = EDGE_CURVE ( 'NONE', #2818, #9323, #12320, .T. ) ;
#12851 = ORIENTED_EDGE ( 'NONE', *, *, #9395, .T. ) ;
#12853 = DIRECTION ( 'NONE',  ( -1.000000000000000000, 0.000000000000000000, -0.000000000000000000 ) ) ;
#12854 = CARTESIAN_POINT ( 'NONE',  ( 0.000000000000000000, 55.51919907100653973, 9.823366686500859757 ) ) ;
#12855 = AXIS2_PLACEMENT_3D ( 'NONE', #1600, #4285, #1688 ) ;
#12856 = EDGE_CURVE ( 'NONE', #10989, #12127, #16609, .T. ) ;
#12857 = DIRECTION ( 'NONE',  ( -1.000000000000000000, 0.000000000000000000, 0.000000000000000000 ) ) ;
#12858 = EDGE_CURVE ( 'NONE', #3875, #2619, #2935, .T. ) ;
#12859 = ADVANCED_FACE ( 'NONE', ( #4206 ), #8206, .F. ) ;
#12860 = EDGE_LOOP ( 'NONE', ( #4300, #10526 ) ) ;
#12861 = EDGE_CURVE ( 'NONE', #475, #7605, #17072, .T. ) ;
#12862 = PRODUCT_DEFINITION_SHAPE ( 'NONE', 'NONE',  #18768 ) ;
#12863 = EDGE_LOOP ( 'NONE', ( #13388, #12190, #14068, #13233 ) ) ;
#12864 = DIRECTION ( 'NONE',  ( 1.000000000000000000, 0.000000000000000000, 0.000000000000000000 ) ) ;
#12865 = CARTESIAN_POINT ( 'NONE',  ( 10.00000000000000000, -55.74967257055887870, 7.478235706488783663 ) ) ;
#12866 = FACE_OUTER_BOUND ( 'NONE', #12468, .T. ) ;
#12867 = DIRECTION ( 'NONE',  ( -1.000000000000000000, -0.000000000000000000, -0.000000000000000000 ) ) ;
#12868 = TOROIDAL_SURFACE ( 'NONE', #17713, 4.000000000000000000, 0.2500000000000000000 ) ;
#12869 = DIRECTION ( 'NONE',  ( -1.000000000000000000, 0.000000000000000000, 0.000000000000000000 ) ) ;
#12871 = AXIS2_PLACEMENT_3D ( 'NONE', #4791, #414, #13470 ) ;
#12870 = CARTESIAN_POINT ( 'NONE',  ( 10.00000000000000000, 49.49802920186223076, 26.71881558261748069 ) ) ;
#12872 = CARTESIAN_POINT ( 'NONE',  ( 4.000000000000000000, -2.309401076758514915, -3.433295621305383349 ) ) ;
#12873 = ORIENTED_EDGE ( 'NONE', *, *, #7016, .F. ) ;
#12874 = CARTESIAN_POINT ( 'NONE',  ( 0.000000000000000000, 0.000000000000000000, 0.000000000000000000 ) ) ;
#12875 = CARTESIAN_POINT ( 'NONE',  ( 0.000000000000000000, 0.000000000000000000, -2.000000000000000000 ) ) ;
#12876 = EDGE_CURVE ( 'NONE', #10185, #421, #18442, .T. ) ;
#12877 = DIRECTION ( 'NONE',  ( 0.000000000000000000, -1.000000000000000000, -1.047444401652940164E-14 ) ) ;
#12878 = CARTESIAN_POINT ( 'NONE',  ( 0.000000000000000000, 15.61693798565582547, -61.03368945066419826 ) ) ;
#12879 = CONTEXT_DEPENDENT_SHAPE_REPRESENTATION ( #16932, #1916 ) ;
#12880 = EDGE_LOOP ( 'NONE', ( #12233, #1456, #5647, #913 ) ) ;
#12881 = ADVANCED_FACE ( 'NONE', ( #5538 ), #11442, .F. ) ;
#12882 = CIRCLE ( 'NONE', #5574, 4.799999999999999822 ) ;
#12883 = AXIS2_PLACEMENT_3D ( 'NONE', #8394, #5627, #7058 ) ;
#12884 = ORIENTED_EDGE ( 'NONE', *, *, #5954, .F. ) ;
#12885 = PLANE ( 'NONE',  #13607 ) ;
#12886 = DIRECTION ( 'NONE',  ( 0.000000000000000000, -1.000000000000000000, -1.040834085585043434E-14 ) ) ;
#12887 = EDGE_LOOP ( 'NONE', ( #7235, #16751 ) ) ;
#12888 = CYLINDRICAL_SURFACE ( 'NONE', #18522, 24.00000000002400213 ) ;
#12889 = EDGE_CURVE ( 'NONE', #5885, #3893, #6964, .T. ) ;
#12890 = FACE_OUTER_BOUND ( 'NONE', #376, .T. ) ;
#12891 = CARTESIAN_POINT ( 'NONE',  ( -90.70833251482494575, -49.14213562373095812, -4.949572208642814886 ) ) ;
#12892 = DIRECTION ( 'NONE',  ( 1.000000000000000000, 0.000000000000000000, 0.000000000000000000 ) ) ;
#12893 = DIRECTION ( 'NONE',  ( 0.000000000000000000, 1.000000000000000000, 0.000000000000000000 ) ) ;
#12894 = ORIENTED_EDGE ( 'NONE', *, *, #18667, .T. ) ;
#12895 = CYLINDRICAL_SURFACE ( 'NONE', #8494, 1.250000000000001110 ) ;
#12896 = ORIENTED_EDGE ( 'NONE', *, *, #4709, .F. ) ;
#12897 = VECTOR ( 'NONE', #7286, 1000.000000000000000 ) ;
#12898 = DIRECTION ( 'NONE',  ( 1.000000000000000000, 0.000000000000000000, 0.000000000000000000 ) ) ;
#12899 = DIRECTION ( 'NONE',  ( -0.000000000000000000, -1.000000000000000000, -0.000000000000000000 ) ) ;
#12900 = ORIENTED_EDGE ( 'NONE', *, *, #12760, .F. ) ;
#12901 = SHAPE_DEFINITION_REPRESENTATION ( #18632, #434 ) ;
#12902 = DIRECTION ( 'NONE',  ( 0.000000000000000000, 0.4539904997395476927, -0.8910065241883673437 ) ) ;
#12903 = ORIENTED_EDGE ( 'NONE', *, *, #14715, .T. ) ;
#12904 = DIRECTION ( 'NONE',  ( 0.000000000000000000, 0.4539904997395479147, -0.8910065241883673437 ) ) ;
#12905 = CARTESIAN_POINT ( 'NONE',  ( 5.000000000000000000, 32.11449294037196722, 54.20017844242522642 ) ) ;
#12906 = CARTESIAN_POINT ( 'NONE',  ( 2.500000000000000000, -2.357898499370431722, 2.818925648462311528E-15 ) ) ;
#12907 = EDGE_CURVE ( 'NONE', #13973, #9150, #11140, .T. ) ;
#12908 = CARTESIAN_POINT ( 'NONE',  ( 0.000000000000000000, -4.381479206522764791, -32.70783759231090926 ) ) ;
#12909 = DIRECTION ( 'NONE',  ( 1.000000000000000000, 0.000000000000000000, 0.000000000000000000 ) ) ;
#12910 = VERTEX_POINT ( 'NONE', #9904 ) ;
#12911 = DIRECTION ( 'NONE',  ( 0.000000000000000000, -1.000000000000000000, 0.000000000000000000 ) ) ;
#12912 = CARTESIAN_POINT ( 'NONE',  ( 0.000000000000000000, -20.41355805489629915, 19.44239304137368407 ) ) ;
#12913 = DIRECTION ( 'NONE',  ( 0.000000000000000000, 0.000000000000000000, 1.000000000000000000 ) ) ;
#12914 = ORIENTED_EDGE ( 'NONE', *, *, #15541, .T. ) ;
#12915 = EDGE_LOOP ( 'NONE', ( #15328, #9212, #15567, #16555 ) ) ;
#12916 = CARTESIAN_POINT ( 'NONE',  ( 5.686050877451574337, -5.768780236673276995, -1.000000000000000000 ) ) ;
#12917 = SURFACE_STYLE_FILL_AREA ( #6046 ) ;
#12918 = MECHANICAL_DESIGN_GEOMETRIC_PRESENTATION_REPRESENTATION (  '', ( #18688 ), #148 ) ;
#12919 = ORIENTED_EDGE ( 'NONE', *, *, #4124, .F. ) ;
#12920 = ADVANCED_FACE ( 'NONE', ( #8660, #10284, #11809, #3233, #14570, #5811, #15, #9032, #7611, #4563, #17348, #8752, #13147 ), #7415, .T. ) ;
#12921 = EDGE_CURVE ( 'NONE', #10165, #596, #4295, .T. ) ;
#12922 = CARTESIAN_POINT ( 'NONE',  ( 0.000000000000000000, -15.68049343256016925, 29.03656532225557996 ) ) ;
#12923 = DIRECTION ( 'NONE',  ( 0.000000000000000000, 0.000000000000000000, 1.000000000000000000 ) ) ;
#12924 = ORIENTED_EDGE ( 'NONE', *, *, #13158, .F. ) ;
#12925 = CARTESIAN_POINT ( 'NONE',  ( 5.000000000000000000, -29.03656532225551601, -15.68049343256028294 ) ) ;
#12926 = AXIS2_PLACEMENT_3D ( 'NONE', #1853, #10889, #15001 ) ;
#12927 = ORIENTED_EDGE ( 'NONE', *, *, #17159, .F. ) ;
#12928 = DIRECTION ( 'NONE',  ( 1.000000000000000000, 0.000000000000000000, 0.000000000000000000 ) ) ;
#12929 = AXIS2_PLACEMENT_3D ( 'NONE', #10091, #14460, #4008 ) ;
#12930 = VERTEX_POINT ( 'NONE', #10098 ) ;
#12931 = CARTESIAN_POINT ( 'NONE',  ( 3.098410542199072637, -7.060458129626440815, -1.000000000000000000 ) ) ;
#12932 = EDGE_LOOP ( 'NONE', ( #316, #9608, #12260, #1270 ) ) ;
#12933 = DIRECTION ( 'NONE',  ( -1.000000000000000000, 0.000000000000000000, 0.000000000000000000 ) ) ;
#12934 = DIRECTION ( 'NONE',  ( -1.000000000000000000, 0.000000000000000000, 0.000000000000000000 ) ) ;
#12935 = ORIENTED_EDGE ( 'NONE', *, *, #1109, .F. ) ;
#12936 = ORIENTED_EDGE ( 'NONE', *, *, #5402, .F. ) ;
#12937 = FACE_OUTER_BOUND ( 'NONE', #5731, .T. ) ;
#12938 = ORIENTED_EDGE ( 'NONE', *, *, #3776, .T. ) ;
#12939 = FACE_OUTER_BOUND ( 'NONE', #3990, .T. ) ;
#12940 = FACE_OUTER_BOUND ( 'NONE', #7767, .T. ) ;
#12941 = PRODUCT_DEFINITION_FORMATION_WITH_SPECIFIED_SOURCE ( 'ANY', '', #9207, .NOT_KNOWN. ) ;
#12942 = AXIS2_PLACEMENT_3D ( 'NONE', #8905, #6143, #6235 ) ;
#12943 = AXIS2_PLACEMENT_3D ( 'NONE', #16230, #3179, #3277 ) ;
#12944 = DIRECTION ( 'NONE',  ( 0.000000000000000000, 0.000000000000000000, 1.000000000000000000 ) ) ;
#12945 = ORIENTED_EDGE ( 'NONE', *, *, #2019, .T. ) ;
#12946 = AXIS2_PLACEMENT_3D ( 'NONE', #4087, #14082, #7984 ) ;
#12947 = ORIENTED_EDGE ( 'NONE', *, *, #1620, .T. ) ;
#12948 = CARTESIAN_POINT ( 'NONE',  ( -1.200950573245989306, -30.00000000000000000, 24.97113769375797787 ) ) ;
#12949 = CARTESIAN_POINT ( 'NONE',  ( 0.000000000000000000, 0.000000000000000000, -4.000000000000000000 ) ) ;
#12950 = CARTESIAN_POINT ( 'NONE',  ( 10.00000000000000000, 47.29147401531953676, 41.62350880771938222 ) ) ;
#12951 = FACE_OUTER_BOUND ( 'NONE', #958, .T. ) ;
#12952 = AXIS2_PLACEMENT_3D ( 'NONE', #13271, #227, #10494 ) ;
#12953 = LINE ( 'NONE', #188, #15162 ) ;
#12954 = LINE ( 'NONE', #4562, #4032 ) ;
#12955 = AXIS2_PLACEMENT_3D ( 'NONE', #7381, #14530, #5864 ) ;
#12956 = CARTESIAN_POINT ( 'NONE',  ( 3.061616997868383043E-15, -30.00000000000000000, -25.00000000000000000 ) ) ;
#12957 = ORIENTED_EDGE ( 'NONE', *, *, #2555, .F. ) ;
#12958 = CARTESIAN_POINT ( 'NONE',  ( 0.02511973781850649831, -4.877415612947427981, -3.751298745799844792 ) ) ;
#12959 = CIRCLE ( 'NONE', #14765, 26.24900000002625333 ) ;
#12960 = EDGE_CURVE ( 'NONE', #7869, #12340, #2618, .T. ) ;
#12961 = EDGE_CURVE ( 'NONE', #1091, #5783, #4655, .T. ) ;
#12962 =( NAMED_UNIT ( * ) PLANE_ANGLE_UNIT ( ) SI_UNIT ( $, .RADIAN. ) );
#12963 = EDGE_CURVE ( 'NONE', #4060, #4800, #9571, .T. ) ;
#12964 = ORIENTED_EDGE ( 'NONE', *, *, #7382, .T. ) ;
#12965 = FACE_OUTER_BOUND ( 'NONE', #17727, .T. ) ;
#12966 = CARTESIAN_POINT ( 'NONE',  ( 34.55500000000001393, 3.061616997868384127E-16, -2.500000000000000888 ) ) ;
#12967 = EDGE_CURVE ( 'NONE', #8010, #8173, #5038, .T. ) ;
#12968 = ORIENTED_EDGE ( 'NONE', *, *, #9189, .T. ) ;
#12969 = CIRCLE ( 'NONE', #12021, 12.00000000001200640 ) ;
#12970 = CIRCLE ( 'NONE', #12653, 63.00000000006298961 ) ;
#12971 = EDGE_CURVE ( 'NONE', #14848, #2085, #10373, .T. ) ;
#12972 = AXIS2_PLACEMENT_3D ( 'NONE', #7833, #3461, #7925 ) ;
#12973 = AXIS2_PLACEMENT_3D ( 'NONE', #11077, #16725, #16901 ) ;
#12974 = AXIS2_PLACEMENT_3D ( 'NONE', #17792, #10559, #6554 ) ;
#12975 = ORIENTED_EDGE ( 'NONE', *, *, #10389, .T. ) ;
#12976 = DIRECTION ( 'NONE',  ( 0.000000000000000000, 0.000000000000000000, -1.000000000000000000 ) ) ;
#12977 = CARTESIAN_POINT ( 'NONE',  ( 0.000000000000000000, 33.95787273855245303, 45.00825343885033192 ) ) ;
#12978 = EDGE_CURVE ( 'NONE', #9150, #6825, #17237, .T. ) ;
#12979 = ORIENTED_EDGE ( 'NONE', *, *, #11350, .F. ) ;
#12980 = CARTESIAN_POINT ( 'NONE',  ( 0.000000000000000000, 0.000000000000000000, 0.000000000000000000 ) ) ;
#12981 = DIRECTION ( 'NONE',  ( -1.000000000000000000, 0.000000000000000000, -0.000000000000000000 ) ) ;
#12982 = CARTESIAN_POINT ( 'NONE',  ( -79.64793068852898728, -38.00000000000000000, -31.86039329588756530 ) ) ;
#12983 = LINE ( 'NONE', #1275, #9160 ) ;
#12984 = AXIS2_PLACEMENT_3D ( 'NONE', #13839, #10785, #12313 ) ;
#12985 = DIRECTION ( 'NONE',  ( 1.000000000000000000, -0.000000000000000000, -0.000000000000000000 ) ) ;
#12986 = ORIENTED_EDGE ( 'NONE', *, *, #3841, .F. ) ;
#12987 = CARTESIAN_POINT ( 'NONE',  ( -17.77999999999999758, 0.000000000000000000, 25.00000000000000000 ) ) ;
#12988 = AXIS2_PLACEMENT_3D ( 'NONE', #2678, #16100, #16188 ) ;
#12989 = ORIENTED_EDGE ( 'NONE', *, *, #12584, .T. ) ;
#12990 = EDGE_CURVE ( 'NONE', #17686, #16356, #5950, .T. ) ;
#12991 = VECTOR ( 'NONE', #16571, 1000.000000000000000 ) ;
#12992 = DIRECTION ( 'NONE',  ( -1.000000000000000000, -0.000000000000000000, 0.000000000000000000 ) ) ;
#12993 = CARTESIAN_POINT ( 'NONE',  ( 10.04305231718605285, -34.99999999999999289, -30.90933677959240811 ) ) ;
#12994 = ORIENTED_EDGE ( 'NONE', *, *, #740, .F. ) ;
#12995 = APPLICATION_PROTOCOL_DEFINITION ( 'draft international standard', 'automotive_design', 1998, #4283 ) ;
#12996 = ORIENTED_EDGE ( 'NONE', *, *, #7018, .T. ) ;
#12997 = EDGE_CURVE ( 'NONE', #5171, #17453, #7328, .T. ) ;
#12998 = AXIS2_PLACEMENT_3D ( 'NONE', #11620, #7324, #17516 ) ;
#12999 = PLANE ( 'NONE',  #15996 ) ;
#13000 = CARTESIAN_POINT ( 'NONE',  ( 21.00000000000000355, 0.000000000000000000, 2.055000000000000160 ) ) ;
#13001 = AXIS2_PLACEMENT_3D ( 'NONE', #4217, #17265, #1175 ) ;
#13002 = AXIS2_PLACEMENT_3D ( 'NONE', #2356, #12458, #18353 ) ;
#13003 = CARTESIAN_POINT ( 'NONE',  ( 0.000000000000000000, 53.29895248911700634, -18.38754094778185788 ) ) ;
#13004 = DIRECTION ( 'NONE',  ( 0.000000000000000000, 0.000000000000000000, 1.000000000000000000 ) ) ;
#13005 = CARTESIAN_POINT ( 'NONE',  ( -26.29305231718568336, -30.00000000000000000, -21.75302069950551953 ) ) ;
#13006 = ORIENTED_EDGE ( 'NONE', *, *, #13877, .F. ) ;
#13007 = CARTESIAN_POINT ( 'NONE',  ( 0.000000000000000000, -18.64666490672410148, 53.06836994729227541 ) ) ;
#13008 = PLANE ( 'NONE',  #3453 ) ;
#13009 = DIRECTION ( 'NONE',  ( 0.000000000000000000, 1.000000000000000000, 0.000000000000000000 ) ) ;
#13010 = AXIS2_PLACEMENT_3D ( 'NONE', #11803, #8840, #14655 ) ;
#13011 = EDGE_LOOP ( 'NONE', ( #14732, #609, #11236, #16449 ) ) ;
#13012 = ORIENTED_EDGE ( 'NONE', *, *, #15782, .T. ) ;
#13013 = CARTESIAN_POINT ( 'NONE',  ( 10.00000000000000000, 0.000000000000000000, 1.500000000000000000 ) ) ;
#13014 = VECTOR ( 'NONE', #612, 1000.000000000000114 ) ;
#13015 = ORIENTED_EDGE ( 'NONE', *, *, #16389, .T. ) ;
#13016 = CIRCLE ( 'NONE', #13323, 56.24900000005626310 ) ;
#13017 = EDGE_CURVE ( 'NONE', #10166, #6265, #5899, .T. ) ;
#13018 = PRODUCT_DEFINITION_SHAPE ( 'NONE', 'NONE',  #18834 ) ;
#13019 = CARTESIAN_POINT ( 'NONE',  ( 5.200000000000002842, 3.306546357697854226E-16, 2.700000000000000622 ) ) ;
#13020 = LINE ( 'NONE', #15789, #3887 ) ;
#13021 = ORIENTED_EDGE ( 'NONE', *, *, #15860, .T. ) ;
#13022 = LINE ( 'NONE', #12925, #10068 ) ;
#13023 = VECTOR ( 'NONE', #3930, 1000.000000000000000 ) ;
#13024 = CIRCLE ( 'NONE', #3910, 63.00000000006298961 ) ;
#13025 = ORIENTED_EDGE ( 'NONE', *, *, #764, .F. ) ;
#13026 = PRODUCT_DEFINITION_CONTEXT ( 'detailed design', #14371, 'design' ) ;
#13027 = DIRECTION ( 'NONE',  ( 0.000000000000000000, 0.000000000000000000, 1.000000000000000000 ) ) ;
#13028 = ORIENTED_EDGE ( 'NONE', *, *, #9471, .F. ) ;
#13029 = ORIENTED_EDGE ( 'NONE', *, *, #8474, .T. ) ;
#13030 = EDGE_CURVE ( 'NONE', #17219, #10404, #16273, .T. ) ;
#13031 = DIRECTION ( 'NONE',  ( 0.000000000000000000, 0.4999999999999992784, -0.8660254037844389297 ) ) ;
#13032 = DIRECTION ( 'NONE',  ( 0.000000000000000000, 0.000000000000000000, 1.000000000000000000 ) ) ;
#13033 = VERTEX_POINT ( 'NONE', #4473 ) ;
#13034 = ORIENTED_EDGE ( 'NONE', *, *, #9776, .T. ) ;
#13035 = DIRECTION ( 'NONE',  ( -1.000000000000000000, -0.000000000000000000, 0.000000000000000000 ) ) ;
#13036 = EDGE_CURVE ( 'NONE', #11369, #15878, #15707, .T. ) ;
#13037 =( NAMED_UNIT ( * ) SI_UNIT ( $, .STERADIAN. ) SOLID_ANGLE_UNIT ( ) );
#13038 = ORIENTED_EDGE ( 'NONE', *, *, #4333, .T. ) ;
#13039 = CARTESIAN_POINT ( 'NONE',  ( -90.00000000009001155, -38.00000000000000000, -27.50000000000000000 ) ) ;
#13040 = CIRCLE ( 'NONE', #3602, 24.00000000002400569 ) ;
#13041 = CIRCLE ( 'NONE', #16984, 24.00000000002400569 ) ;
#13042=STYLED_ITEM('',(#18883),#15898);
#13043 = AXIS2_PLACEMENT_3D ( 'NONE', #7689, #12268, #15511 ) ;
#13044 = DIRECTION ( 'NONE',  ( 1.000000000000000000, 0.000000000000000000, 0.000000000000000000 ) ) ;
#13045 = ORIENTED_EDGE ( 'NONE', *, *, #9102, .T. ) ;
#13046 = AXIS2_PLACEMENT_3D ( 'NONE', #14795, #1747, #4794 ) ;
#13047 = ORIENTED_EDGE ( 'NONE', *, *, #6440, .F. ) ;
#13048 = DIRECTION ( 'NONE',  ( -1.000000000000000000, 0.000000000000000000, 0.000000000000000000 ) ) ;
#13049 = DIRECTION ( 'NONE',  ( 0.000000000000000000, 0.000000000000000000, 1.000000000000000000 ) ) ;
#13050 = CARTESIAN_POINT ( 'NONE',  ( -90.00000000009001155, -38.00000000000000000, -1.301042606982603940E-15 ) ) ;
#13051 = DIRECTION ( 'NONE',  ( 0.000000000000000000, -1.287488025362403787E-15, -1.000000000000000000 ) ) ;
#13052 = DIRECTION ( 'NONE',  ( 0.000000000000000000, 0.8090169943749486725, -0.5877852522924714718 ) ) ;
#13053 = CIRCLE ( 'NONE', #5442, 2.100000000000000089 ) ;
#13054 = DIRECTION ( 'NONE',  ( -1.000000000000000000, -0.000000000000000000, -0.000000000000000000 ) ) ;
#13055 = CARTESIAN_POINT ( 'NONE',  ( 3.673940397442059178E-15, 10.00000000000000000, 30.00000000000000000 ) ) ;
#13056 = VECTOR ( 'NONE', #14963, 1000.000000000000000 ) ;
#13057 = LINE ( 'NONE', #13337, #8996 ) ;
#13058 = ORIENTED_EDGE ( 'NONE', *, *, #1328, .F. ) ;
#13059 = DIRECTION ( 'NONE',  ( 0.000000000000000000, 0.000000000000000000, 1.000000000000000000 ) ) ;
#13060 =( NAMED_UNIT ( * ) SI_UNIT ( $, .STERADIAN. ) SOLID_ANGLE_UNIT ( ) );
#13061 = ORIENTED_EDGE ( 'NONE', *, *, #3883, .F. ) ;
#13062 = FACE_OUTER_BOUND ( 'NONE', #18662, .T. ) ;
#13063 = CARTESIAN_POINT ( 'NONE',  ( -11.25000000000000533, 3.667817163446322894E-15, -29.90000000000000213 ) ) ;
#13064 = VERTEX_POINT ( 'NONE', #1428 ) ;
#13065 = AXIS2_PLACEMENT_3D ( 'NONE', #6768, #5148, #680 ) ;
#13066 = AXIS2_PLACEMENT_3D ( 'NONE', #10444, #14550, #14733 ) ;
#13067 = EDGE_CURVE ( 'NONE', #16371, #4390, #13057, .T. ) ;
#13068 = ORIENTED_EDGE ( 'NONE', *, *, #11101, .T. ) ;
#13069 = FACE_BOUND ( 'NONE', #1068, .T. ) ;
#13070 = EDGE_CURVE ( 'NONE', #15596, #13860, #5271, .T. ) ;
#13071 = CARTESIAN_POINT ( 'NONE',  ( 0.000000000000000000, -19.44239304137390434, 20.41355805489607889 ) ) ;
#13072 = ORIENTED_EDGE ( 'NONE', *, *, #15862, .F. ) ;
#13073 = CARTESIAN_POINT ( 'NONE',  ( 0.000000000000000000, 1.305124410222461284, -2.000000000000000000 ) ) ;
#13074 = DIRECTION ( 'NONE',  ( -1.000000000000000000, 0.000000000000000000, 0.000000000000000000 ) ) ;
#13075 = PRODUCT_DEFINITION ( 'UNKNOWN', '', #773, #13026 ) ;
#13076 = CARTESIAN_POINT ( 'NONE',  ( 3.499999999999999556, -27.60846790388774608, -2.000000000000000000 ) ) ;
#13077 = AXIS2_PLACEMENT_3D ( 'NONE', #12777, #1059, #5620 ) ;
#13078 = CARTESIAN_POINT ( 'NONE',  ( 10.00000000000000000, -55.33199130079790962, 10.11537145609357502 ) ) ;
#13079 = DIRECTION ( 'NONE',  ( 1.000000000000000000, 0.000000000000000000, 0.000000000000000000 ) ) ;
#13080 = ORIENTED_EDGE ( 'NONE', *, *, #2247, .F. ) ;
#13081 = CARTESIAN_POINT ( 'NONE',  ( -90.00000000009001155, -29.99899999999999878, -10.00000000000001066 ) ) ;
#13082 = ORIENTED_EDGE ( 'NONE', *, *, #3655, .T. ) ;
#13083 = AXIS2_PLACEMENT_3D ( 'NONE', #12734, #14154, #12538 ) ;
#13084 = ADVANCED_FACE ( 'NONE', ( #12361 ), #6176, .F. ) ;
#13085 = FACE_BOUND ( 'NONE', #9911, .T. ) ;
#13086 = DIRECTION ( 'NONE',  ( 0.000000000000000000, 0.000000000000000000, 1.000000000000000000 ) ) ;
#13087 = ORIENTED_EDGE ( 'NONE', *, *, #15947, .T. ) ;
#13088 = CONTEXT_DEPENDENT_SHAPE_REPRESENTATION ( #3306, #16523 ) ;
#13089 = ORIENTED_EDGE ( 'NONE', *, *, #5110, .T. ) ;
#13090 = EDGE_CURVE ( 'NONE', #15420, #9197, #810, .T. ) ;
#13091 = CIRCLE ( 'NONE', #929, 63.00000000006298961 ) ;
#13092 = ADVANCED_FACE ( 'NONE', ( #3423 ), #7982, .T. ) ;
#13093 = VERTEX_POINT ( 'NONE', #12081 ) ;
#13094 = AXIS2_PLACEMENT_3D ( 'NONE', #3675, #17862, #12148 ) ;
#13095 = CARTESIAN_POINT ( 'NONE',  ( -90.00000000009001155, 1.828182762038084424E-14, -1.561251128379122243E-15 ) ) ;
#13096 = ADVANCED_FACE ( 'NONE', ( #14947 ), #4938, .F. ) ;
#13097 = DIRECTION ( 'NONE',  ( 0.000000000000000000, 0.5000000000000011102, 0.8660254037844379305 ) ) ;
#13098 = ADVANCED_BREP_SHAPE_REPRESENTATION ( '', ( #15935, #8017 ), #15633 ) ;
#13099 = DIRECTION ( 'NONE',  ( 1.000000000000000000, 0.000000000000000000, 0.000000000000000000 ) ) ;
#13100 = DIRECTION ( 'NONE',  ( 0.000000000000000000, 0.000000000000000000, 1.000000000000000000 ) ) ;
#13101 = EDGE_CURVE ( 'NONE', #10254, #3708, #7789, .T. ) ;
#13102 = DIRECTION ( 'NONE',  ( -2.031314180040284764E-16, -1.000000000000000000, -1.301042606982601377E-16 ) ) ;
#13103 = VERTEX_POINT ( 'NONE', #16658 ) ;
#13104 = EDGE_CURVE ( 'NONE', #2993, #11781, #6184, .T. ) ;
#13105 = DIRECTION ( 'NONE',  ( 0.000000000000000000, 0.000000000000000000, 1.000000000000000000 ) ) ;
#13106 = CARTESIAN_POINT ( 'NONE',  ( 5.000000000000000000, 47.29147401531955097, 41.62350880771938222 ) ) ;
#13107 = DIRECTION ( 'NONE',  ( -1.000000000000000000, -0.000000000000000000, -0.000000000000000000 ) ) ;
#13108 = EDGE_LOOP ( 'NONE', ( #15791, #1795, #14635, #5469 ) ) ;
#13109 = VERTEX_POINT ( 'NONE', #5019 ) ;
#13110 = DIRECTION ( 'NONE',  ( 0.000000000000000000, 0.000000000000000000, 1.000000000000000000 ) ) ;
#13111 = AXIS2_PLACEMENT_3D ( 'NONE', #17656, #10408, #7552 ) ;
#13112 = CARTESIAN_POINT ( 'NONE',  ( 0.000000000000000000, 0.000000000000000000, 0.000000000000000000 ) ) ;
#13113 = VERTEX_POINT ( 'NONE', #9217 ) ;
#13114 = DIRECTION ( 'NONE',  ( 0.000000000000000000, 1.000000000000000000, 0.000000000000000000 ) ) ;
#13115 = DIRECTION ( 'NONE',  ( -1.000000000000000000, -0.000000000000000000, -0.000000000000000000 ) ) ;
#13116 = DIRECTION ( 'NONE',  ( 1.000000000000000000, 0.000000000000000000, 0.000000000000000000 ) ) ;
#13117 = VERTEX_POINT ( 'NONE', #3618 ) ;
#13119 = VECTOR ( 'NONE', #6001, 1000.000000000000000 ) ;
#13118 = CARTESIAN_POINT ( 'NONE',  ( 4.000000000000000000, 2.309401076758515803, -0.4999999999999995559 ) ) ;
#13120 = ORIENTED_EDGE ( 'NONE', *, *, #8191, .F. ) ;
#13121 = DIRECTION ( 'NONE',  ( 0.000000000000000000, 0.000000000000000000, 1.000000000000000000 ) ) ;
#13122 = VERTEX_POINT ( 'NONE', #4747 ) ;
#13123 = EDGE_CURVE ( 'NONE', #5795, #4060, #13618, .T. ) ;
#13124 = ORIENTED_EDGE ( 'NONE', *, *, #13318, .T. ) ;
#13125 = DIRECTION ( 'NONE',  ( 0.000000000000000000, 0.000000000000000000, -1.000000000000000000 ) ) ;
#13126 = CARTESIAN_POINT ( 'NONE',  ( 10.00000000000000178, 6.123233995736766282E-16, -5.000000000000000000 ) ) ;
#13127 = ORIENTED_EDGE ( 'NONE', *, *, #4418, .T. ) ;
#13128 = ORIENTED_EDGE ( 'NONE', *, *, #1280, .T. ) ;
#13129 = CYLINDRICAL_SURFACE ( 'NONE', #14205, 20.00000000000000000 ) ;
#13130 = SURFACE_SIDE_STYLE ('',( #5883 ) ) ;
#13131 = VERTEX_POINT ( 'NONE', #13796 ) ;
#13132 = DIRECTION ( 'NONE',  ( 0.000000000000000000, 0.000000000000000000, 1.000000000000000000 ) ) ;
#13133 = AXIS2_PLACEMENT_3D ( 'NONE', #2148, #10708, #5280 ) ;
#13134 = VECTOR ( 'NONE', #9925, 1000.000000000000000 ) ;
#13135 = LINE ( 'NONE', #7317, #74 ) ;
#13136 = VECTOR ( 'NONE', #10939, 1000.000000000000227 ) ;
#13137 = VERTEX_POINT ( 'NONE', #13516 ) ;
#13138 = ORIENTED_EDGE ( 'NONE', *, *, #15543, .T. ) ;
#13139 = CARTESIAN_POINT ( 'NONE',  ( -82.50000000008999734, -13.00000000000001954, -5.777138986694822120E-16 ) ) ;
#13140 = DIRECTION ( 'NONE',  ( 0.000000000000000000, -0.000000000000000000, 1.000000000000000000 ) ) ;
#13141 = CARTESIAN_POINT ( 'NONE',  ( 2.250000000000000000, -27.60846790388774608, -2.000000000000000000 ) ) ;
#13142 = VERTEX_POINT ( 'NONE', #1981 ) ;
#13143 = CARTESIAN_POINT ( 'NONE',  ( -4.000000000000000000, 2.471528634177585282, -3.686887442155186712 ) ) ;
#13144 = ADVANCED_FACE ( 'NONE', ( #15037 ), #15233, .T. ) ;
#13145 = DIRECTION ( 'NONE',  ( 0.000000000000000000, 0.000000000000000000, 1.000000000000000000 ) ) ;
#13146 = FACE_OUTER_BOUND ( 'NONE', #16075, .T. ) ;
#13147 = FACE_BOUND ( 'NONE', #12271, .T. ) ;
#13148 = EDGE_LOOP ( 'NONE', ( #312, #18180, #8436, #18242 ) ) ;
#13149 = DIRECTION ( 'NONE',  ( 0.000000000000000000, 0.000000000000000000, 1.000000000000000000 ) ) ;
#13150 = DIRECTION ( 'NONE',  ( -1.000000000000000000, 0.000000000000000000, 0.000000000000000000 ) ) ;
#13151 = AXIS2_PLACEMENT_3D ( 'NONE', #1, #18749, #12857 ) ;
#13152 = VERTEX_POINT ( 'NONE', #566 ) ;
#13153 = CARTESIAN_POINT ( 'NONE',  ( -36.40576474687271258, 10.00000000000000000, -26.45033635316118747 ) ) ;
#13154 = FACE_OUTER_BOUND ( 'NONE', #8397, .T. ) ;
#13155 = APPLICATION_CONTEXT ( 'automotive_design' ) ;
#13156 = EDGE_CURVE ( 'NONE', #13103, #15464, #9615, .T. ) ;
#13157 = ORIENTED_EDGE ( 'NONE', *, *, #11721, .T. ) ;
#13158 = EDGE_CURVE ( 'NONE', #6241, #1304, #15057, .T. ) ;
#13159 = CARTESIAN_POINT ( 'NONE',  ( 0.000000000000000000, 0.000000000000000000, -1.000000000000000000 ) ) ;
#13160 = CARTESIAN_POINT ( 'NONE',  ( 0.000000000000000000, 0.000000000000000000, 0.000000000000000000 ) ) ;
#13161 = EDGE_LOOP ( 'NONE', ( #12666, #9735, #16716, #8468 ) ) ;
#13162 = DIRECTION ( 'NONE',  ( -0.000000000000000000, -1.000000000000000000, -0.000000000000000000 ) ) ;
#13163 = CARTESIAN_POINT ( 'NONE',  ( -3.309651814758565180, -5.455921364805393026, -1.000000000000000000 ) ) ;
#13164 = CYLINDRICAL_SURFACE ( 'NONE', #9659, 63.00000000006298961 ) ;
#13165 = DIRECTION ( 'NONE',  ( -1.000000000000000000, 0.000000000000000000, -0.000000000000000000 ) ) ;
#13166 = CARTESIAN_POINT ( 'NONE',  ( 10.00000000000000000, 0.000000000000000000, 0.000000000000000000 ) ) ;
#13167 = VERTEX_POINT ( 'NONE', #16554 ) ;
#13168 = DIRECTION ( 'NONE',  ( 1.000000000000000000, 0.000000000000000000, -0.000000000000000000 ) ) ;
#13169 = EDGE_LOOP ( 'NONE', ( #1601, #13223, #10114, #1459, #5824, #16737, #1780, #9285, #692, #855, #13387, #2236, #14070, #3638, #12873, #4589, #4262, #3796, #13636, #5244, #150, #12784, #11493, #709, #17507, #17321, #10767, #17492, #4684, #17595, #15413, #2094, #11311, #17797, #14907, #1485, #13982, #8080, #16003, #11149, #15725, #11916, #10851, #5816, #14537, #7898, #11446, #4723, #15859, #13762, #8670, #16983, #14340, #13589, #14872, #12728, #6846, #13545, #8107, #18495, #17118, #11215, #5889, #10616, #18733, #13613, #14485, #9374, #13831, #12935, #11688, #1526, #7335, #14002, #15127, #11066, #16507, #14396, #17334, #16709, #8177, #15014, #8281, #10054, #11850, #370, #9367, #97, #1194, #3981, #8138, #9752, #1614, #18386, #11500, #1114, #18048, #6752, #7075, #16348, #10835, #17309, #11605, #15963, #15891, #5423, #4545, #15617, #9144, #4332, #12577, #7983, #6326, #3866, #10259, #12280, #6848, #5284, #14937, #8581, #17082, #13758, #14920, #9863, #13187, #15223, #10555, #9673, #5603, #17594, #5510, #12201, #2204, #670, #18398, #2506, #2444, #16381, #15301, #17544, #4339, #2234, #12896, #15802, #7407, #171, #10999, #16797, #13399, #10396, #15715, #17402, #10320, #16481, #14081, #2920, #1844, #9424, #14835, #17677, #7790, #2113, #3164, #11300, #1977 ) ) ;
#13170 = PRODUCT_DEFINITION_SHAPE ( 'NONE', 'NONE',  #18827 ) ;
#13171 = DIRECTION ( 'NONE',  ( -1.000000000000000000, 0.000000000000000000, 0.000000000000000000 ) ) ;
#13172 = DIRECTION ( 'NONE',  ( 0.000000000000000000, 0.3090169943749480619, -0.9510565162951533091 ) ) ;
#13173 = ORIENTED_EDGE ( 'NONE', *, *, #8650, .F. ) ;
#13174 = AXIS2_PLACEMENT_3D ( 'NONE', #11604, #17409, #4361 ) ;
#13175 = ORIENTED_EDGE ( 'NONE', *, *, #42, .F. ) ;
#13176 = CIRCLE ( 'NONE', #6162, 23.50000000000001066 ) ;
#13177 = AXIS2_PLACEMENT_3D ( 'NONE', #14016, #975, #12679 ) ;
#13178 = DIRECTION ( 'NONE',  ( 0.000000000000000000, 0.9876883405951383255, -0.1564344650402276493 ) ) ;
#13179 = LINE ( 'NONE', #1474, #18262 ) ;
#13180 = EDGE_CURVE ( 'NONE', #18103, #2724, #6843, .T. ) ;
#13181 = CARTESIAN_POINT ( 'NONE',  ( 5.000000000000000000, 5.940243314904670946, -32.46095361140686464 ) ) ;
#13182 = CARTESIAN_POINT ( 'NONE',  ( 10.00000000000000000, 0.000000000000000000, 0.000000000000000000 ) ) ;
#13183 = CIRCLE ( 'NONE', #7703, 56.24900000005625600 ) ;
#13184 = CARTESIAN_POINT ( 'NONE',  ( -12.50000000000000533, 3.429011037612589670E-15, 28.00000000000000355 ) ) ;
#13185 = DIRECTION ( 'NONE',  ( -1.000000000000000000, 0.000000000000000000, 0.000000000000000000 ) ) ;
#13186 = CARTESIAN_POINT ( 'NONE',  ( 0.000000000000000000, 16.60877409751168798, 20.32630374611190760 ) ) ;
#13187 = ORIENTED_EDGE ( 'NONE', *, *, #11819, .F. ) ;
#13188 = DIRECTION ( 'NONE',  ( -0.000000000000000000, -0.000000000000000000, 1.000000000000000000 ) ) ;
#13189 = CARTESIAN_POINT ( 'NONE',  ( 10.00000000000000000, -16.60877409751182654, 20.32630374611179391 ) ) ;
#13190 = DIRECTION ( 'NONE',  ( -1.000000000000000000, 0.000000000000000000, 0.000000000000000000 ) ) ;
#13191 = ORIENTED_EDGE ( 'NONE', *, *, #12013, .F. ) ;
#13192 = ORIENTED_EDGE ( 'NONE', *, *, #12997, .F. ) ;
#13193 = ADVANCED_FACE ( 'NONE', ( #9097 ), #10521, .T. ) ;
#13194 = EDGE_CURVE ( 'NONE', #13575, #3711, #247, .T. ) ;
#13195 = DIRECTION ( 'NONE',  ( 0.000000000000000000, -1.000000000000000000, 0.000000000000000000 ) ) ;
#13196 = EDGE_CURVE ( 'NONE', #5299, #11990, #2585, .T. ) ;
#13197 = EDGE_LOOP ( 'NONE', ( #8345, #15361, #8011, #6294 ) ) ;
#13198 = ADVANCED_FACE ( 'NONE', ( #3020 ), #4535, .F. ) ;
#13199 = ADVANCED_FACE ( 'NONE', ( #3199 ), #69, .T. ) ;
#13200 = FACE_BOUND ( 'NONE', #17407, .T. ) ;
#13201 = DIRECTION ( 'NONE',  ( 0.000000000000000000, 0.000000000000000000, -1.000000000000000000 ) ) ;
#13202 = CARTESIAN_POINT ( 'NONE',  ( 10.00000000000000000, 55.83748330407408389, -7.813799127873475747 ) ) ;
#13203 = ORIENTED_EDGE ( 'NONE', *, *, #10187, .F. ) ;
#13204 = CARTESIAN_POINT ( 'NONE',  ( -290.0000000000001137, -34.99999999999999289, -125.0000000000000000 ) ) ;
#13205 = EDGE_CURVE ( 'NONE', #15093, #13701, #14916, .T. ) ;
#13206 = ORIENTED_EDGE ( 'NONE', *, *, #15426, .F. ) ;
#13207 = DIRECTION ( 'NONE',  ( 1.000000000000000000, 0.000000000000000000, 0.000000000000000000 ) ) ;
#13208 = ORIENTED_EDGE ( 'NONE', *, *, #14036, .F. ) ;
#13209 = ORIENTED_EDGE ( 'NONE', *, *, #1576, .F. ) ;
#13210 = COLOUR_RGB ( '',1.000000000000000000, 0.9490196078431372140, 0.9098039215686274384 ) ;
#13211 = DIRECTION ( 'NONE',  ( -1.000000000000000000, 0.000000000000000000, 0.000000000000000000 ) ) ;
#13212 = DIRECTION ( 'NONE',  ( -1.000000000000000000, -0.000000000000000000, -0.000000000000000000 ) ) ;
#13213 = VERTEX_POINT ( 'NONE', #4347 ) ;
#13214 = ORIENTED_EDGE ( 'NONE', *, *, #12687, .T. ) ;
#13215 = ADVANCED_FACE ( 'NONE', ( #16342 ), #1493, .T. ) ;
#13216 = CARTESIAN_POINT ( 'NONE',  ( 0.000000000000000000, -1.335003989222025123, 56.23315539212689629 ) ) ;
#13217 =( NAMED_UNIT ( * ) PLANE_ANGLE_UNIT ( ) SI_UNIT ( $, .RADIAN. ) );
#13218 = ORIENTED_EDGE ( 'NONE', *, *, #9578, .T. ) ;
#13219 = CARTESIAN_POINT ( 'NONE',  ( 10.00000000000000000, 0.000000000000000000, 0.000000000000000000 ) ) ;
#13220 = EDGE_CURVE ( 'NONE', #72, #13484, #7383, .T. ) ;
#13221 = COLOUR_RGB ( '',1.000000000000000000, 0.9490196078431372140, 0.9098039215686274384 ) ;
#13222 = CARTESIAN_POINT ( 'NONE',  ( -12.69999999999999929, 0.000000000000000000, 0.000000000000000000 ) ) ;
#13223 = ORIENTED_EDGE ( 'NONE', *, *, #13687, .F. ) ;
#13224 = ORIENTED_EDGE ( 'NONE', *, *, #6313, .T. ) ;
#13225 = CARTESIAN_POINT ( 'NONE',  ( -31.74999999999995737, 0.000000000000000000, 2.500000000000000444 ) ) ;
#13226 = DIRECTION ( 'NONE',  ( 0.000000000000000000, 0.000000000000000000, 1.000000000000000000 ) ) ;
#13227 = CARTESIAN_POINT ( 'NONE',  ( 0.000000000000000000, 0.000000000000000000, 0.000000000000000000 ) ) ;
#13228 = ORIENTED_EDGE ( 'NONE', *, *, #12861, .F. ) ;
#13229 = DIRECTION ( 'NONE',  ( 1.000000000000000000, 0.000000000000000000, 0.000000000000000000 ) ) ;
#13230 = DIRECTION ( 'NONE',  ( 0.000000000000000000, 0.000000000000000000, 1.000000000000000000 ) ) ;
#13231 = CYLINDRICAL_SURFACE ( 'NONE', #2810, 56.24900000005625600 ) ;
#13232 = DIRECTION ( 'NONE',  ( 0.000000000000000000, -1.000000000000000000, 0.000000000000000000 ) ) ;
#13233 = ORIENTED_EDGE ( 'NONE', *, *, #9575, .T. ) ;
#13234 = CARTESIAN_POINT ( 'NONE',  ( 10.00000000000000000, 14.19907017806868588, 22.07705612348844326 ) ) ;
#13235 = CARTESIAN_POINT ( 'NONE',  ( 0.000000000000000000, 0.000000000000000000, 0.000000000000000000 ) ) ;
#13236 = DIRECTION ( 'NONE',  ( 0.000000000000000000, 0.3090169943749479509, -0.9510565162951533091 ) ) ;
#13237 = ORIENTED_EDGE ( 'NONE', *, *, #6384, .F. ) ;
#13238 = DIRECTION ( 'NONE',  ( -0.000000000000000000, 1.000000000000000000, -0.000000000000000000 ) ) ;
#13239 = CARTESIAN_POINT ( 'NONE',  ( 0.5000000000000000000, -6.429618962271402616, 0.000000000000000000 ) ) ;
#13240 = AXIS2_PLACEMENT_3D ( 'NONE', #7296, #17760, #11678 ) ;
#13241 = AXIS2_PLACEMENT_3D ( 'NONE', #5468, #1079, #6985 ) ;
#13242 = EDGE_CURVE ( 'NONE', #12431, #11050, #6240, .T. ) ;
#13243 = EDGE_LOOP ( 'NONE', ( #16071, #1832, #13214, #16668 ) ) ;
#13244 = DIRECTION ( 'NONE',  ( -1.000000000000000000, 0.000000000000000000, -0.000000000000000000 ) ) ;
#13245 = CARTESIAN_POINT ( 'NONE',  ( 10.00000000000000000, -24.33982105418865061, -50.71018745830470920 ) ) ;
#13246 = AXIS2_PLACEMENT_3D ( 'NONE', #7472, #13295, #10519 ) ;
#13247 = EDGE_LOOP ( 'NONE', ( #9774, #1262, #3765, #18385 ) ) ;
#13248 = CARTESIAN_POINT ( 'NONE',  ( -6.259644161404860030E-16, -4.618802153517027165, -3.433295621305388234 ) ) ;
#13249 = CIRCLE ( 'NONE', #17808, 27.50000000000000000 ) ;
#13250 = PLANE ( 'NONE',  #10226 ) ;
#13251 = DIRECTION ( 'NONE',  ( -1.000000000000000000, -0.000000000000000000, -0.000000000000000000 ) ) ;
#13252 = CARTESIAN_POINT ( 'NONE',  ( 0.1481481481481481122, -4.797713218419819903, -1.000000000000000000 ) ) ;
#13253 = CARTESIAN_POINT ( 'NONE',  ( 4.999999999999999112, 32.46095361140700675, -5.940243314903876026 ) ) ;
#13254 = ORIENTED_EDGE ( 'NONE', *, *, #7851, .F. ) ;
#13255 = LINE ( 'NONE', #6012, #7878 ) ;
#13256 = ORIENTED_EDGE ( 'NONE', *, *, #6811, .T. ) ;
#13257 = EDGE_CURVE ( 'NONE', #8847, #14291, #775, .T. ) ;
#13258 =( NAMED_UNIT ( * ) PLANE_ANGLE_UNIT ( ) SI_UNIT ( $, .RADIAN. ) );
#13259 = CARTESIAN_POINT ( 'NONE',  ( 1.567478505476134606E-15, 4.618802153517012066, -3.433295621305382905 ) ) ;
#13260 = EDGE_LOOP ( 'NONE', ( #4942, #10993, #16263, #2361 ) ) ;
#13261 = APPLICATION_PROTOCOL_DEFINITION ( 'draft international standard', 'automotive_design', 1998, #12172 ) ;
#13262 = ADVANCED_FACE ( 'NONE', ( #11953 ), #12007, .T. ) ;
#13263 = CARTESIAN_POINT ( 'NONE',  ( -5.032868406504333869, -28.36021363089093938, -2.000000000000000000 ) ) ;
#13264 = ORIENTED_EDGE ( 'NONE', *, *, #14210, .F. ) ;
#13265 = CIRCLE ( 'NONE', #8112, 56.24900000005625600 ) ;
#13266 = AXIS2_PLACEMENT_3D ( 'NONE', #14854, #369, #4381 ) ;
#13267 = CARTESIAN_POINT ( 'NONE',  ( -290.0000000000001705, -34.99999999999999289, 125.0000000000000000 ) ) ;
#13268 = CARTESIAN_POINT ( 'NONE',  ( 0.000000000000000000, 50.69000562871642046, 24.68609584167177218 ) ) ;
#13269 = AXIS2_PLACEMENT_3D ( 'NONE', #3632, #9806, #6849 ) ;
#13270 = COLOUR_RGB ( '',1.000000000000000000, 0.9490196078431372140, 0.9098039215686274384 ) ;
#13271 = CARTESIAN_POINT ( 'NONE',  ( -79.64793068852927149, -30.00000000000000000, 31.86039329588764701 ) ) ;
#13272 = CARTESIAN_POINT ( 'NONE',  ( -2.000000000000000000, -6.429618962271402616, -1.000000000000000000 ) ) ;
#13273 = AXIS2_PLACEMENT_3D ( 'NONE', #8861, #2978, #13356 ) ;
#13274 = FACE_OUTER_BOUND ( 'NONE', #2441, .T. ) ;
#13275 = CARTESIAN_POINT ( 'NONE',  ( -9.345251662538453630, -28.92794965710190525, -2.000000000000000000 ) ) ;
#13276 = VECTOR ( 'NONE', #8312, 999.9999999999997726 ) ;
#13277 = CARTESIAN_POINT ( 'NONE',  ( 10.00000000000000000, 32.70783759231085952, 4.381479206523099634 ) ) ;
#13278 = AXIS2_PLACEMENT_3D ( 'NONE', #18247, #5195, #6724 ) ;
#13279 = DIRECTION ( 'NONE',  ( 0.000000000000000000, 0.000000000000000000, 1.000000000000000000 ) ) ;
#13280 = EDGE_LOOP ( 'NONE', ( #7112, #18602 ) ) ;
#13281 = DIRECTION ( 'NONE',  ( -0.000000000000000000, 1.000000000000000000, -0.000000000000000000 ) ) ;
#13282 = DIRECTION ( 'NONE',  ( -0.000000000000000000, 1.000000000000000000, -0.000000000000000000 ) ) ;
#13283 = DIRECTION ( 'NONE',  ( 0.000000000000000000, 0.4539904997395412534, 0.8910065241883705633 ) ) ;
#13284 = VERTEX_POINT ( 'NONE', #5865 ) ;
#13285 = ORIENTED_EDGE ( 'NONE', *, *, #15721, .F. ) ;
#13286 =( REPRESENTATION_RELATIONSHIP ('NONE','NONE', #11014, #8256 ) REPRESENTATION_RELATIONSHIP_WITH_TRANSFORMATION ( #16583 )SHAPE_REPRESENTATION_RELATIONSHIP( ) );
#13287 = CARTESIAN_POINT ( 'NONE',  ( 4.999999999999999112, -24.97244012287460535, -57.83923611457346681 ) ) ;
#13288 = LINE ( 'NONE', #18653, #12539 ) ;
#13289 = VERTEX_POINT ( 'NONE', #153 ) ;
#13290 = AXIS2_PLACEMENT_3D ( 'NONE', #15030, #9025, #182 ) ;
#13291 = VECTOR ( 'NONE', #7034, 1000.000000000000000 ) ;
#13292 = CIRCLE ( 'NONE', #14497, 0.7499999999999997780 ) ;
#13293 = AXIS2_PLACEMENT_3D ( 'NONE', #4667, #11821, #8945 ) ;
#13294 = AXIS2_PLACEMENT_3D ( 'NONE', #18520, #14233, #12902 ) ;
#13295 = DIRECTION ( 'NONE',  ( -1.000000000000000000, -0.000000000000000000, 0.000000000000000000 ) ) ;
#13296 = CARTESIAN_POINT ( 'NONE',  ( 1.360585162435110629, -4.061296242128317857, -3.505054077164905024 ) ) ;
#13297 = CARTESIAN_POINT ( 'NONE',  ( 10.00000000000000000, -16.60877409751153522, -20.32630374611203194 ) ) ;
#13298 = ORIENTED_EDGE ( 'NONE', *, *, #12793, .T. ) ;
#13299 = EDGE_CURVE ( 'NONE', #364, #7035, #1072, .T. ) ;
#13300 = DIRECTION ( 'NONE',  ( 1.000000000000000000, 0.000000000000000000, 0.000000000000000000 ) ) ;
#13301 = EDGE_CURVE ( 'NONE', #9087, #125, #17480, .T. ) ;
#13302 = AXIS2_PLACEMENT_3D ( 'NONE', #12075, #17699, #13706 ) ;
#13303 = ORIENTED_EDGE ( 'NONE', *, *, #10793, .T. ) ;
#13304 = DIRECTION ( 'NONE',  ( -1.000000000000000000, 0.000000000000000000, -0.000000000000000000 ) ) ;
#13305 = ORIENTED_EDGE ( 'NONE', *, *, #9291, .T. ) ;
#13306 = AXIS2_PLACEMENT_3D ( 'NONE', #10556, #2173, #17984 ) ;
#13307 = ADVANCED_FACE ( 'NONE', ( #11863 ), #13350, .F. ) ;
#13308 = CARTESIAN_POINT ( 'NONE',  ( 0.000000000000000000, 0.000000000000000000, 0.000000000000000000 ) ) ;
#13309 = DIRECTION ( 'NONE',  ( 0.000000000000000000, -1.000000000000000000, 0.000000000000000000 ) ) ;
#13310 = CIRCLE ( 'NONE', #15745, 2.041999999999999815 ) ;
#13311 = EDGE_LOOP ( 'NONE', ( #11279, #16599, #5548, #7841 ) ) ;
#13312 = ORIENTED_EDGE ( 'NONE', *, *, #746, .F. ) ;
#13313 = CIRCLE ( 'NONE', #17561, 63.00000000006298961 ) ;
#13314 = FACE_OUTER_BOUND ( 'NONE', #16534, .T. ) ;
#13315 = EDGE_CURVE ( 'NONE', #10477, #17054, #4732, .T. ) ;
#13316 = ORIENTED_EDGE ( 'NONE', *, *, #17653, .T. ) ;
#13317 = CYLINDRICAL_SURFACE ( 'NONE', #282, 56.24900000005625600 ) ;
#13318 = EDGE_CURVE ( 'NONE', #16201, #7161, #2785, .T. ) ;
#13319 = VECTOR ( 'NONE', #14540, 1000.000000000000000 ) ;
#13320 = AXIS2_PLACEMENT_3D ( 'NONE', #3472, #16515, #9175 ) ;
#13321 = CARTESIAN_POINT ( 'NONE',  ( 3.522875095019493141, -2.820352903225631369, -3.598441714920572299 ) ) ;
#13322 = CIRCLE ( 'NONE', #15761, 24.00000000002399858 ) ;
#13323 = AXIS2_PLACEMENT_3D ( 'NONE', #18395, #12794, #5256 ) ;
#13324 = ORIENTED_EDGE ( 'NONE', *, *, #8643, .T. ) ;
#13325 = EDGE_CURVE ( 'NONE', #262, #4831, #15368, .T. ) ;
#13326 = EDGE_CURVE ( 'NONE', #11258, #11551, #10488, .T. ) ;
#13327 = ORIENTED_EDGE ( 'NONE', *, *, #11451, .T. ) ;
#13328 = CARTESIAN_POINT ( 'NONE',  ( 10.00000000000000000, 0.000000000000000000, 0.000000000000000000 ) ) ;
#13329 = DIRECTION ( 'NONE',  ( -1.000000000000000000, 0.000000000000000000, 0.000000000000000000 ) ) ;
#13330 = CARTESIAN_POINT ( 'NONE',  ( -10.00000000000000000, 42.79754323328179311, -16.55576474687299537 ) ) ;
#13331 = ORIENTED_EDGE ( 'NONE', *, *, #12961, .T. ) ;
#13332 = CARTESIAN_POINT ( 'NONE',  ( -3.999999999998910649, -1.658469974638591804, -3.531532913075256186 ) ) ;
#13333 = EDGE_CURVE ( 'NONE', #5713, #5418, #6232, .T. ) ;
#13334 = CYLINDRICAL_SURFACE ( 'NONE', #17603, 2.649999999999992806 ) ;
#13335 = CARTESIAN_POINT ( 'NONE',  ( 0.000000000000000000, 0.000000000000000000, 0.000000000000000000 ) ) ;
#13336 = AXIS2_PLACEMENT_3D ( 'NONE', #9283, #539, #7582 ) ;
#13337 = CARTESIAN_POINT ( 'NONE',  ( 5.000000000000000000, 33.71303790549275448, 53.22058882792209289 ) ) ;
#13338 = ORIENTED_EDGE ( 'NONE', *, *, #9153, .T. ) ;
#13339 = FACE_OUTER_BOUND ( 'NONE', #9055, .T. ) ;
#13340 = ADVANCED_FACE ( 'NONE', ( #3410 ), #6363, .T. ) ;
#13341 = FILL_AREA_STYLE ('',( #11895 ) ) ;
#13342 = AXIS2_PLACEMENT_3D ( 'NONE', #11274, #14499, #13172 ) ;
#13343 = ORIENTED_EDGE ( 'NONE', *, *, #13416, .T. ) ;
#13344 = DIRECTION ( 'NONE',  ( -1.000000000000000000, -0.000000000000000000, 0.000000000000000000 ) ) ;
#13345 = CARTESIAN_POINT ( 'NONE',  ( 10.04305231718605285, -34.99999999999999289, -28.25933677959240953 ) ) ;
#13346 = CIRCLE ( 'NONE', #13952, 56.24900000005625600 ) ;
#13347 = AXIS2_PLACEMENT_3D ( 'NONE', #3813, #15436, #2387 ) ;
#13348 = VERTEX_POINT ( 'NONE', #11880 ) ;
#13349 = CIRCLE ( 'NONE', #2706, 24.00000000002399858 ) ;
#13350 =( BOUNDED_SURFACE ( )  B_SPLINE_SURFACE ( 3, 2, ( 
 ( #1858, #11773, #7661 ),
 ( #10344, #16155, #17675 ),
 ( #14718, #1667, #13296 ),
 ( #10445, #3499, #7774 ),
 ( #13602, #13697, #13321 ),
 ( #9298, #16457, #552 ) ),
 .UNSPECIFIED., .F., .F., .F. ) 
 B_SPLINE_SURFACE_WITH_KNOTS ( ( 4, 2, 4 ),
 ( 3, 3 ),
 ( 0.02032853247518126918, 0.02278863295364821906, 0.02524873343211517240 ),
 ( 0.000000000000000000, 1.000000000000000000 ),
 .UNSPECIFIED. ) 
 GEOMETRIC_REPRESENTATION_ITEM ( )  RATIONAL_B_SPLINE_SURFACE ( (
 ( 1.000000000000000000, 0.8047781615896837382, 1.000000000000000000),
 ( 1.000000000000000000, 0.8123767586289252218, 1.000000000000000000),
 ( 1.000000000000000000, 0.8190662415564388121, 1.000000000000000000),
 ( 1.000000000000000000, 0.8192361015669026303, 1.000000000000000000),
 ( 1.000000000000000000, 0.8126135807103900266, 1.000000000000000000),
 ( 1.000000000000000000, 0.8047712338318593339, 1.000000000000000000) ) ) 
 REPRESENTATION_ITEM ( '' )  SURFACE ( )  );
#13351 = FACE_OUTER_BOUND ( 'NONE', #346, .T. ) ;
#13352 = CARTESIAN_POINT ( 'NONE',  ( -290.0000000000001705, -34.99999999999999289, 125.0000000000000000 ) ) ;
#13353 = CIRCLE ( 'NONE', #13960, 33.00000000003299760 ) ;
#13354 = ORIENTED_EDGE ( 'NONE', *, *, #6095, .F. ) ;
#13355 = CARTESIAN_POINT ( 'NONE',  ( -1.149515148933674504E-15, -4.647091401871393579, -3.572172305156879890 ) ) ;
#13356 = DIRECTION ( 'NONE',  ( 0.000000000000000000, 0.000000000000000000, 1.000000000000000000 ) ) ;
#13357 = DIRECTION ( 'NONE',  ( 0.000000000000000000, 0.000000000000000000, 1.000000000000000000 ) ) ;
#13358 = CYLINDRICAL_SURFACE ( 'NONE', #973, 33.00000000003299760 ) ;
#13359 = CARTESIAN_POINT ( 'NONE',  ( -79.64793068852927149, -30.00000000000000000, 29.21039329588765554 ) ) ;
#13360 = ORIENTED_EDGE ( 'NONE', *, *, #18080, .F. ) ;
#13361 = DIRECTION ( 'NONE',  ( 0.000000000000000000, 0.000000000000000000, 1.000000000000000000 ) ) ;
#13362 = VERTEX_POINT ( 'NONE', #16366 ) ;
#13363 = EDGE_CURVE ( 'NONE', #10074, #808, #10193, .T. ) ;
#13364 = CARTESIAN_POINT ( 'NONE',  ( -4.207491450040567571, 2.029819825146470524, -3.671670828759566074 ) ) ;
#13365 = CIRCLE ( 'NONE', #10617, 5.000000000000004441 ) ;
#13366 = VERTEX_POINT ( 'NONE', #18061 ) ;
#13367 = AXIS2_PLACEMENT_3D ( 'NONE', #14287, #9987, #1242 ) ;
#13368 = EDGE_LOOP ( 'NONE', ( #10908, #7921, #1232, #18583 ) ) ;
#13369 = ORIENTED_EDGE ( 'NONE', *, *, #12534, .T. ) ;
#13370 = VERTEX_POINT ( 'NONE', #6255 ) ;
#13371 = ADVANCED_FACE ( 'NONE', ( #4925 ), #5005, .T. ) ;
#13372 = FACE_OUTER_BOUND ( 'NONE', #3751, .T. ) ;
#13373 = CARTESIAN_POINT ( 'NONE',  ( -79.64793068852898728, -30.00000000000000000, -34.51039329588756033 ) ) ;
#13374 = AXIS2_PLACEMENT_3D ( 'NONE', #11248, #11542, #15911 ) ;
#13375 = CARTESIAN_POINT ( 'NONE',  ( 2.500000000000000000, 1.178949249685212974, -2.042000000000001148 ) ) ;
#13376 = DIRECTION ( 'NONE',  ( -1.000000000000000000, -0.000000000000000000, -0.000000000000000000 ) ) ;
#13377 = CIRCLE ( 'NONE', #14897, 2.649999999999985700 ) ;
#13378 = EDGE_CURVE ( 'NONE', #3895, #9120, #3204, .T. ) ;
#13379 = DIRECTION ( 'NONE',  ( 1.000000000000000000, -0.000000000000000000, -0.000000000000000000 ) ) ;
#13380 = CARTESIAN_POINT ( 'NONE',  ( 10.00000000000000000, 42.79754323328179311, -11.25576474687299644 ) ) ;
#13381 = CYLINDRICAL_SURFACE ( 'NONE', #12943, 12.00000000001200462 ) ;
#13382 = LINE ( 'NONE', #6128, #3934 ) ;
#13383 = ORIENTED_EDGE ( 'NONE', *, *, #11741, .T. ) ;
#13384 = CYLINDRICAL_SURFACE ( 'NONE', #17819, 63.00000000006298961 ) ;
#13385 = CYLINDRICAL_SURFACE ( 'NONE', #1930, 26.24900000002624978 ) ;
#13386 = CARTESIAN_POINT ( 'NONE',  ( 0.000000000000000000, 15.68049343255996675, 29.03656532225569009 ) ) ;
#13387 = ORIENTED_EDGE ( 'NONE', *, *, #13674, .F. ) ;
#13388 = ORIENTED_EDGE ( 'NONE', *, *, #13606, .F. ) ;
#13389 = CARTESIAN_POINT ( 'NONE',  ( 0.000000000000000000, -26.45033635316118747, 39.05576474687271116 ) ) ;
#13390 = DIRECTION ( 'NONE',  ( 0.000000000000000000, 0.000000000000000000, 1.000000000000000000 ) ) ;
#13391 = DIRECTION ( 'NONE',  ( -1.000000000000000000, 0.000000000000000000, -0.000000000000000000 ) ) ;
#13392 = EDGE_LOOP ( 'NONE', ( #11834, #535, #12848, #594, #14922, #12287, #15582, #15016 ) ) ;
#13393 = CIRCLE ( 'NONE', #15522, 26.24900000002624978 ) ;
#13394 = VECTOR ( 'NONE', #10134, 1000.000000000000000 ) ;
#13395 = EDGE_CURVE ( 'NONE', #8897, #3688, #449, .T. ) ;
#13396 = CARTESIAN_POINT ( 'NONE',  ( 0.000000000000000000, -12.18267823974732522, -25.42247726998028057 ) ) ;
#13397 = CARTESIAN_POINT ( 'NONE',  ( 2.500000000000000000, -1.178949249685214307, 2.042000000000001592 ) ) ;
#13398 = CARTESIAN_POINT ( 'NONE',  ( -2.000000000000000000, -6.429618962271402616, -1.000000000000000000 ) ) ;
#13399 = ORIENTED_EDGE ( 'NONE', *, *, #16189, .F. ) ;
#13400 = DIRECTION ( 'NONE',  ( 0.000000000000000000, -0.9876883405951359940, -0.1564344650402419989 ) ) ;
#13401 = EDGE_CURVE ( 'NONE', #538, #1960, #14840, .T. ) ;
#13402 = ORIENTED_EDGE ( 'NONE', *, *, #4923, .F. ) ;
#13403 = CIRCLE ( 'NONE', #5184, 28.00000000000000355 ) ;
#13404 = FACE_OUTER_BOUND ( 'NONE', #8286, .T. ) ;
#13405 = ORIENTED_EDGE ( 'NONE', *, *, #18657, .F. ) ;
#13406 = AXIS2_PLACEMENT_3D ( 'NONE', #7171, #7640, #3554 ) ;
#13407 = DIRECTION ( 'NONE',  ( -0.000000000000000000, 1.000000000000000000, -0.000000000000000000 ) ) ;
#13408 = CARTESIAN_POINT ( 'NONE',  ( -2.725741868435985094, 3.045094352034055429, -3.220599429844047012 ) ) ;
#13409 = ORIENTED_EDGE ( 'NONE', *, *, #8193, .T. ) ;
#13410 = ORIENTED_EDGE ( 'NONE', *, *, #10591, .T. ) ;
#13411 = DIRECTION ( 'NONE',  ( -0.000000000000000000, 1.000000000000000000, -0.000000000000000000 ) ) ;
#13412 =( NAMED_UNIT ( * ) PLANE_ANGLE_UNIT ( ) SI_UNIT ( $, .RADIAN. ) );
#13413 = ORIENTED_EDGE ( 'NONE', *, *, #11346, .F. ) ;
#13414 = CARTESIAN_POINT ( 'NONE',  ( 10.00000000000000000, 55.51919907100666762, -9.823366686500051514 ) ) ;
#13415 = EDGE_CURVE ( 'NONE', #10818, #17139, #12066, .T. ) ;
#13416 = EDGE_CURVE ( 'NONE', #91, #15064, #18097, .T. ) ;
#13417 = AXIS2_PLACEMENT_3D ( 'NONE', #10113, #17714, #15922 ) ;
#13418 = DIRECTION ( 'NONE',  ( -1.000000000000000000, -0.000000000000000000, -0.000000000000000000 ) ) ;
#13419 = ORIENTED_EDGE ( 'NONE', *, *, #1360, .T. ) ;
#13420 = EDGE_LOOP ( 'NONE', ( #10131, #12219, #10592, #3318 ) ) ;
#13421 = CARTESIAN_POINT ( 'NONE',  ( -4.000000000000000000, 0.000000000000000000, 0.000000000000000000 ) ) ;
#13422 = CARTESIAN_POINT ( 'NONE',  ( 10.00000000000000000, -29.75305054077461975, -14.27431201565556940 ) ) ;
#13423 = LINE ( 'NONE', #10733, #4481 ) ;
#13424 = ORIENTED_EDGE ( 'NONE', *, *, #16455, .F. ) ;
#13425 = CYLINDRICAL_SURFACE ( 'NONE', #12389, 12.00000000001200462 ) ;
#13426 = CARTESIAN_POINT ( 'NONE',  ( 2.000000000000005329, -3.464101615137751722, 0.000000000000000000 ) ) ;
#13427 = FACE_BOUND ( 'NONE', #4404, .T. ) ;
#13428 = DIRECTION ( 'NONE',  ( -1.000000000000000000, 0.000000000000000000, -0.000000000000000000 ) ) ;
#13429 = EDGE_LOOP ( 'NONE', ( #1040, #7862, #634, #3015 ) ) ;
#13430 = DIRECTION ( 'NONE',  ( -0.000000000000000000, 1.000000000000000000, -0.000000000000000000 ) ) ;
#13431 =( NAMED_UNIT ( * ) PLANE_ANGLE_UNIT ( ) SI_UNIT ( $, .RADIAN. ) );
#13432 = ORIENTED_EDGE ( 'NONE', *, *, #71, .F. ) ;
#13433 = DIRECTION ( 'NONE',  ( -1.000000000000000000, -0.000000000000000000, 0.000000000000000000 ) ) ;
#13434 = CARTESIAN_POINT ( 'NONE',  ( 0.000000000000000000, 32.46095361140700675, -5.940243314903877803 ) ) ;
#13435 = ADVANCED_FACE ( 'NONE', ( #1878 ), #7679, .T. ) ;
#13436 = EDGE_CURVE ( 'NONE', #12710, #4722, #15962, .T. ) ;
#13437 = EDGE_CURVE ( 'NONE', #4084, #5247, #939, .T. ) ;
#13438 = EDGE_CURVE ( 'NONE', #15353, #16371, #4117, .T. ) ;
#13439 = EDGE_CURVE ( 'NONE', #4430, #17584, #9582, .T. ) ;
#13440 = EDGE_LOOP ( 'NONE', ( #14723, #11408, #10232, #3380 ) ) ;
#13441 = CARTESIAN_POINT ( 'NONE',  ( 0.000000000000000000, -5.120903701083534543E-13, -45.00000000000000000 ) ) ;
#13442 = ORIENTED_EDGE ( 'NONE', *, *, #7749, .F. ) ;
#13443 = CARTESIAN_POINT ( 'NONE',  ( 2.500000000000000000, 2.357898499370432166, -2.385244779468109755E-15 ) ) ;
#13444 = LINE ( 'NONE', #18193, #216 ) ;
#13445 = EDGE_CURVE ( 'NONE', #2692, #6586, #5637, .T. ) ;
#13446 = CIRCLE ( 'NONE', #14956, 26.24900000002624978 ) ;
#13447 = VECTOR ( 'NONE', #18367, 1000.000000000000000 ) ;
#13448 = CYLINDRICAL_SURFACE ( 'NONE', #7549, 2.649999999999995914 ) ;
#13449 = CARTESIAN_POINT ( 'NONE',  ( 0.000000000000000000, 3.000000000000000000, 0.000000000000000000 ) ) ;
#13450 = DIRECTION ( 'NONE',  ( -0.000000000000000000, 1.000000000000000000, -0.000000000000000000 ) ) ;
#13451 = VERTEX_POINT ( 'NONE', #6925 ) ;
#13452 = LINE ( 'NONE', #11734, #11547 ) ;
#13453 = ORIENTED_EDGE ( 'NONE', *, *, #12094, .F. ) ;
#13454 = DIRECTION ( 'NONE',  ( 1.000000000000000000, 0.000000000000000000, 0.000000000000000000 ) ) ;
#13455 = CARTESIAN_POINT ( 'NONE',  ( 10.00000000000000000, 26.49895292618076326, -49.76630880786279931 ) ) ;
#13456 = ORIENTED_EDGE ( 'NONE', *, *, #15532, .F. ) ;
#13457 = EDGE_CURVE ( 'NONE', #179, #7917, #8373, .T. ) ;
#13458 = ITEM_DEFINED_TRANSFORMATION ( 'NONE', 'NONE', #448,  #8017 ) ;
#13459 = EDGE_LOOP ( 'NONE', ( #10127, #930, #853, #11775 ) ) ;
#13460 = SHAPE_REPRESENTATION ( 'spur gear_iso_ISO - Spur gear 3M 20T 20PA 10FW ---S20A75H50L10.0S1', ( #8017 ), #11074 ) ;
#13461 = CIRCLE ( 'NONE', #10111, 24.00000000002399858 ) ;
#13462 = ORIENTED_EDGE ( 'NONE', *, *, #1665, .T. ) ;
#13463 = EDGE_CURVE ( 'NONE', #3123, #7777, #2889, .T. ) ;
#13464 = ORIENTED_EDGE ( 'NONE', *, *, #5234, .F. ) ;
#13465 = CARTESIAN_POINT ( 'NONE',  ( 10.00000000000000000, 0.000000000000000000, 0.000000000000000000 ) ) ;
#13466 = FACE_OUTER_BOUND ( 'NONE', #3679, .T. ) ;
#13467 = DIRECTION ( 'NONE',  ( -1.000000000000000000, 0.000000000000000000, 0.000000000000000000 ) ) ;
#13468 = CARTESIAN_POINT ( 'NONE',  ( 11.14999999999999680, 0.000000000000000000, 25.10000000000000142 ) ) ;
#13469 = LINE ( 'NONE', #6410, #1150 ) ;
#13470 = DIRECTION ( 'NONE',  ( 0.000000000000000000, 0.000000000000000000, 1.000000000000000000 ) ) ;
#13471 = CYLINDRICAL_SURFACE ( 'NONE', #10489, 24.00000000002400213 ) ;
#13472 = FACE_OUTER_BOUND ( 'NONE', #13368, .T. ) ;
#13473 = ORIENTED_EDGE ( 'NONE', *, *, #11272, .T. ) ;
#13474 = CIRCLE ( 'NONE', #1901, 12.00000000001200462 ) ;
#13475 = DIRECTION ( 'NONE',  ( -1.000000000000000000, -0.000000000000000000, 0.000000000000000000 ) ) ;
#13476 = FACE_OUTER_BOUND ( 'NONE', #3779, .T. ) ;
#13477 = DIRECTION ( 'NONE',  ( 0.000000000000000000, 0.000000000000000000, 1.000000000000000000 ) ) ;
#13478 = EDGE_LOOP ( 'NONE', ( #15360, #16670, #6459, #5183 ) ) ;
#13479 = EDGE_LOOP ( 'NONE', ( #15801, #2207, #4259, #12096, #18235 ) ) ;
#13480 = CIRCLE ( 'NONE', #15910, 4.250000000000000000 ) ;
#13481 = DIRECTION ( 'NONE',  ( -1.000000000000000000, -0.000000000000000000, -0.000000000000000000 ) ) ;
#13482 = CARTESIAN_POINT ( 'NONE',  ( -26.29305231718584324, -21.50000000000000000, 19.10302069950530779 ) ) ;
#13483 = CARTESIAN_POINT ( 'NONE',  ( 10.00000000000000000, 7.813799127873274131, 55.83748330407410521 ) ) ;
#13484 = VERTEX_POINT ( 'NONE', #18545 ) ;
#13485 = PRODUCT_DEFINITION_SHAPE ( 'NONE', 'NONE',  #4673 ) ;
#13486 = EDGE_CURVE ( 'NONE', #17410, #11328, #12634, .T. ) ;
#13487 = FACE_OUTER_BOUND ( 'NONE', #16659, .T. ) ;
#13488 = DIRECTION ( 'NONE',  ( 0.000000000000000000, 0.000000000000000000, 1.000000000000000000 ) ) ;
#13489 = AXIS2_PLACEMENT_3D ( 'NONE', #4944, #378, #3431 ) ;
#13490 = DIRECTION ( 'NONE',  ( -1.000000000000000000, -0.000000000000000000, 0.000000000000000000 ) ) ;
#13491 = EDGE_LOOP ( 'NONE', ( #7159, #7682, #5726, #5552 ) ) ;
#13492 = DIRECTION ( 'NONE',  ( -1.000000000000000000, 0.000000000000000000, 0.000000000000000000 ) ) ;
#13493 = VERTEX_POINT ( 'NONE', #5401 ) ;
#13494 = DIRECTION ( 'NONE',  ( -1.000000000000000000, -0.000000000000000000, -0.000000000000000000 ) ) ;
#13495 = EDGE_LOOP ( 'NONE', ( #400, #1399, #15937, #1636 ) ) ;
#13496 = DIRECTION ( 'NONE',  ( 0.000000000000000000, 0.000000000000000000, 1.000000000000000000 ) ) ;
#13497 = DIRECTION ( 'NONE',  ( -1.000000000000000000, 0.000000000000000000, 0.000000000000000000 ) ) ;
#13498 = ORIENTED_EDGE ( 'NONE', *, *, #16346, .F. ) ;
#13499 = EDGE_LOOP ( 'NONE', ( #2071, #1776, #10351 ) ) ;
#13500 = EDGE_CURVE ( 'NONE', #7210, #16278, #7747, .T. ) ;
#13501 = DIRECTION ( 'NONE',  ( 0.000000000000000000, 0.000000000000000000, -1.000000000000000000 ) ) ;
#13502 = EDGE_LOOP ( 'NONE', ( #4618, #7874 ) ) ;
#13503 = DIRECTION ( 'NONE',  ( 0.000000000000000000, 0.000000000000000000, 1.000000000000000000 ) ) ;
#13504 = EDGE_CURVE ( 'NONE', #6017, #17166, #15307, .T. ) ;
#13505 = CARTESIAN_POINT ( 'NONE',  ( -90.00000000009001155, -88.00000000000000000, -1.301042606982603940E-15 ) ) ;
#13506 = ORIENTED_EDGE ( 'NONE', *, *, #383, .T. ) ;
#13507 = VECTOR ( 'NONE', #14598, 1000.000000000000000 ) ;
#13508 = ORIENTED_EDGE ( 'NONE', *, *, #13934, .T. ) ;
#13509 = CARTESIAN_POINT ( 'NONE',  ( -12.69999999999999929, 0.000000000000000000, -28.00000000000000355 ) ) ;
#13510 = CARTESIAN_POINT ( 'NONE',  ( 10.00000000000000000, 50.71018745830478736, -24.33982105418846942 ) ) ;
#13511 = DIRECTION ( 'NONE',  ( -1.000000000000000000, 0.000000000000000000, -0.000000000000000000 ) ) ;
#13512 = VERTEX_POINT ( 'NONE', #6733 ) ;
#13513 = LINE ( 'NONE', #11977, #11782 ) ;
#13514 = CARTESIAN_POINT ( 'NONE',  ( 4.000000000000000000, -2.309401076758516691, -0.4999999999999995559 ) ) ;
#13515 = FACE_OUTER_BOUND ( 'NONE', #15471, .T. ) ;
#13516 = CARTESIAN_POINT ( 'NONE',  ( 0.000000000000000000, -5.876895005582878362, 62.72529079327805590 ) ) ;
#13517 = ORIENTED_EDGE ( 'NONE', *, *, #1291, .F. ) ;
#13518 = DIRECTION ( 'NONE',  ( 0.000000000000000000, -0.9510565162951565288, 0.3090169943749382364 ) ) ;
#13519 = DIRECTION ( 'NONE',  ( 0.000000000000000000, -0.9510565162951564178, 0.3090169943749384585 ) ) ;
#13520 = VERTEX_POINT ( 'NONE', #6821 ) ;
#13521 = CARTESIAN_POINT ( 'NONE',  ( 0.000000000000000000, -55.83748330407401284, -7.813799127873885197 ) ) ;
#13522 = LINE ( 'NONE', #15044, #14395 ) ;
#13523 = ADVANCED_BREP_SHAPE_REPRESENTATION ( '', ( #15898, #8017 ), #2572 ) ;
#13524 = EDGE_LOOP ( 'NONE', ( #3750, #14596, #15938, #11026 ) ) ;
#13525 = DIRECTION ( 'NONE',  ( 1.000000000000000000, -0.000000000000000000, -0.000000000000000000 ) ) ;
#13526 = ORIENTED_EDGE ( 'NONE', *, *, #14737, .F. ) ;
#13527 =( NAMED_UNIT ( * ) PLANE_ANGLE_UNIT ( ) SI_UNIT ( $, .RADIAN. ) );
#13528 = EDGE_CURVE ( 'NONE', #17453, #13370, #10507, .T. ) ;
#13529 = DIRECTION ( 'NONE',  ( -0.000000000000000000, 1.000000000000000000, -0.000000000000000000 ) ) ;
#13530 = EDGE_CURVE ( 'NONE', #16959, #14039, #9682, .T. ) ;
#13531 = MECHANICAL_DESIGN_GEOMETRIC_PRESENTATION_REPRESENTATION (  '', ( #3801 ), #1069 ) ;
#13532 = EDGE_CURVE ( 'NONE', #15320, #5321, #8086, .T. ) ;
#13533 = CYLINDRICAL_SURFACE ( 'NONE', #7243, 2.649999999999992806 ) ;
#13534 = DIRECTION ( 'NONE',  ( -1.000000000000000000, -0.000000000000000000, -0.000000000000000000 ) ) ;
#13535 = VECTOR ( 'NONE', #9018, 1000.000000000000000 ) ;
#13536 = CARTESIAN_POINT ( 'NONE',  ( 10.00000000000000000, 56.37237871411035428, -1.017308535511785683 ) ) ;
#13537 = ORIENTED_EDGE ( 'NONE', *, *, #8130, .T. ) ;
#13538 = CARTESIAN_POINT ( 'NONE',  ( -79.64793068852898728, -34.99999999999999289, -34.51039329588756033 ) ) ;
#13539 = CIRCLE ( 'NONE', #5318, 26.24900000002624978 ) ;
#13540 = ADVANCED_FACE ( 'NONE', ( #18258 ), #8264, .F. ) ;
#13541 =( NAMED_UNIT ( * ) SI_UNIT ( $, .STERADIAN. ) SOLID_ANGLE_UNIT ( ) );
#13542 = CYLINDRICAL_SURFACE ( 'NONE', #14177, 2.649999999999999467 ) ;
#13543 = ORIENTED_EDGE ( 'NONE', *, *, #3309, .T. ) ;
#13544 = EDGE_CURVE ( 'NONE', #14160, #1567, #18444, .T. ) ;
#13545 = ORIENTED_EDGE ( 'NONE', *, *, #17599, .F. ) ;
#13546 = EDGE_CURVE ( 'NONE', #17956, #4897, #1393, .T. ) ;
#13547 = DIRECTION ( 'NONE',  ( -1.000000000000000000, 0.000000000000000000, 0.000000000000000000 ) ) ;
#13548 = ORIENTED_EDGE ( 'NONE', *, *, #15764, .F. ) ;
#13549 = ADVANCED_FACE ( 'NONE', ( #741 ), #6644, .F. ) ;
#13550 = CIRCLE ( 'NONE', #13246, 56.24900000005625600 ) ;
#13551 = ORIENTED_EDGE ( 'NONE', *, *, #14822, .F. ) ;
#13552 = DIRECTION ( 'NONE',  ( -1.000000000000000000, -0.000000000000000000, 0.000000000000000000 ) ) ;
#13553 = LINE ( 'NONE', #18110, #17060 ) ;
#13554 = DIRECTION ( 'NONE',  ( -1.000000000000000000, 0.000000000000000000, 0.000000000000000000 ) ) ;
#13555 = DIRECTION ( 'NONE',  ( 0.000000000000000000, 0.000000000000000000, 1.000000000000000000 ) ) ;
#13556 = ADVANCED_FACE ( 'NONE', ( #16834 ), #3783, .T. ) ;
#13557 = EDGE_CURVE ( 'NONE', #806, #17177, #1685, .T. ) ;
#13558 = DIRECTION ( 'NONE',  ( 0.000000000000000000, -0.5000000000000011102, -0.8660254037844379305 ) ) ;
#13559 = PLANE ( 'NONE',  #5866 ) ;
#13560 = CIRCLE ( 'NONE', #6565, 24.00000000002399858 ) ;
#13561 = DIRECTION ( 'NONE',  ( -1.000000000000000000, 0.000000000000000000, 0.000000000000000000 ) ) ;
#13562 = VERTEX_POINT ( 'NONE', #1392 ) ;
#13563 = FACE_OUTER_BOUND ( 'NONE', #14998, .T. ) ;
#13564 = ORIENTED_EDGE ( 'NONE', *, *, #2646, .F. ) ;
#13565 = CARTESIAN_POINT ( 'NONE',  ( 0.000000000000000000, 0.000000000000000000, 0.000000000000000000 ) ) ;
#13566 = CARTESIAN_POINT ( 'NONE',  ( -290.0000000000001705, -34.99999999999999289, 125.0000000000000000 ) ) ;
#13567 = EDGE_LOOP ( 'NONE', ( #18462, #8541, #11981, #13058 ) ) ;
#13568 = VECTOR ( 'NONE', #4409, 1000.000000000000000 ) ;
#13569 = VERTEX_POINT ( 'NONE', #1492 ) ;
#13570 = CIRCLE ( 'NONE', #15380, 12.00000000001200640 ) ;
#13571 = ADVANCED_FACE ( 'NONE', ( #14430 ), #12830, .T. ) ;
#13572 = FACE_OUTER_BOUND ( 'NONE', #3785, .T. ) ;
#13573 = DIRECTION ( 'NONE',  ( 1.000000000000000000, 0.000000000000000000, 0.000000000000000000 ) ) ;
#13574 = DIRECTION ( 'NONE',  ( 0.000000000000000000, 0.9876883405951371042, 0.1564344650402347547 ) ) ;
#13575 = VERTEX_POINT ( 'NONE', #4431 ) ;
#13576 = CIRCLE ( 'NONE', #10534, 26.24900000002624978 ) ;
#13577 = AXIS2_PLACEMENT_3D ( 'NONE', #17569, #10332, #7459 ) ;
#13578 = CIRCLE ( 'NONE', #816, 12.00000000001200817 ) ;
#13579 = CARTESIAN_POINT ( 'NONE',  ( -90.00000000009001155, 1.000000000000014655, -5.000000000000005329 ) ) ;
#13580 = FACE_OUTER_BOUND ( 'NONE', #14269, .T. ) ;
#13581 = AXIS2_PLACEMENT_3D ( 'NONE', #10112, #15834, #4308 ) ;
#13582 = TOROIDAL_SURFACE ( 'NONE', #493, 25.10000000000000142, 0.09999999999999853451 ) ;
#13584 = AXIS2_PLACEMENT_3D ( 'NONE', #17617, #14661, #1525 ) ;
#13583 = CYLINDRICAL_SURFACE ( 'NONE', #12698, 4.799999999999999822 ) ;
#13585 = ORIENTED_EDGE ( 'NONE', *, *, #17302, .F. ) ;
#13586 = DIRECTION ( 'NONE',  ( 0.000000000000000000, 0.000000000000000000, 1.000000000000000000 ) ) ;
#13587 = ORIENTED_EDGE ( 'NONE', *, *, #16440, .T. ) ;
#13588 = LINE ( 'NONE', #10530, #17002 ) ;
#13589 = ORIENTED_EDGE ( 'NONE', *, *, #1066, .F. ) ;
#13590 = DIRECTION ( 'NONE',  ( 0.000000000000000000, 0.000000000000000000, 1.000000000000000000 ) ) ;
#13591 = CARTESIAN_POINT ( 'NONE',  ( 0.000000000000000000, -26.45033635316118747, 36.40576474687271258 ) ) ;
#13592 = VECTOR ( 'NONE', #10647, 1000.000000000000000 ) ;
#13593 = EDGE_LOOP ( 'NONE', ( #14443, #10978, #8836, #1314 ) ) ;
#13594 = EDGE_LOOP ( 'NONE', ( #6392, #11292 ) ) ;
#13595 = EDGE_CURVE ( 'NONE', #478, #11596, #7197, .T. ) ;
#13596 = FACE_OUTER_BOUND ( 'NONE', #452, .T. ) ;
#13597 = CIRCLE ( 'NONE', #9022, 56.24900000005625600 ) ;
#13598 = ORIENTED_EDGE ( 'NONE', *, *, #1656, .T. ) ;
#13599 = CYLINDRICAL_SURFACE ( 'NONE', #10635, 33.00000000003299760 ) ;
#13600 = VECTOR ( 'NONE', #3553, 999.9999999999998863 ) ;
#13601 = CIRCLE ( 'NONE', #5073, 24.00000000002399858 ) ;
#13602 = CARTESIAN_POINT ( 'NONE',  ( 3.455068668934414777, -2.624017327439094327, -3.316620875263732504 ) ) ;
#13603 = AXIS2_PLACEMENT_3D ( 'NONE', #10366, #8838, #14653 ) ;
#13604 = ORIENTED_EDGE ( 'NONE', *, *, #7521, .F. ) ;
#13605 = AXIS2_PLACEMENT_3D ( 'NONE', #1035, #18357, #5306 ) ;
#13606 = EDGE_CURVE ( 'NONE', #6586, #10475, #15785, .T. ) ;
#13607 = AXIS2_PLACEMENT_3D ( 'NONE', #6099, #14671, #8856 ) ;
#13608 = EDGE_LOOP ( 'NONE', ( #9516, #5645, #61, #15527 ) ) ;
#13609 = LINE ( 'NONE', #13225, #17555 ) ;
#13610 = VECTOR ( 'NONE', #3464, 1000.000000000000000 ) ;
#13611 = LINE ( 'NONE', #8175, #5000 ) ;
#13612 = DIRECTION ( 'NONE',  ( 0.000000000000000000, -0.9876883405951358830, -0.1564344650402420822 ) ) ;
#13613 = ORIENTED_EDGE ( 'NONE', *, *, #10454, .F. ) ;
#13614 = CARTESIAN_POINT ( 'NONE',  ( 1.567478505476134606E-15, 4.618802153517012066, -3.433295621305382905 ) ) ;
#13615 = EDGE_CURVE ( 'NONE', #15064, #9000, #3520, .T. ) ;
#13616 = DIRECTION ( 'NONE',  ( 1.000000000000000000, 0.000000000000000000, 0.000000000000000000 ) ) ;
#13617 = FACE_OUTER_BOUND ( 'NONE', #10586, .T. ) ;
#13618 = LINE ( 'NONE', #9311, #11996 ) ;
#13619 = ORIENTED_EDGE ( 'NONE', *, *, #4687, .F. ) ;
#13620 = DIRECTION ( 'NONE',  ( -1.000000000000000000, 0.000000000000000000, 0.000000000000000000 ) ) ;
#13621 = EDGE_LOOP ( 'NONE', ( #1364, #14058 ) ) ;
#13622 = FACE_OUTER_BOUND ( 'NONE', #10298, .T. ) ;
#13623 = CARTESIAN_POINT ( 'NONE',  ( 0.000000000000000000, 26.20671763660628528, 1.489278925039608570 ) ) ;
#13624 = AXIS2_PLACEMENT_3D ( 'NONE', #17786, #4738, #10554 ) ;
#13625 = AXIS2_PLACEMENT_3D ( 'NONE', #8976, #7844, #13666 ) ;
#13626 = AXIS2_PLACEMENT_3D ( 'NONE', #2431, #9662, #8245 ) ;
#13627 = VECTOR ( 'NONE', #7258, 1000.000000000000000 ) ;
#13628 = ORIENTED_EDGE ( 'NONE', *, *, #14720, .T. ) ;
#13629 = AXIS2_PLACEMENT_3D ( 'NONE', #18424, #5283, #13964 ) ;
#13630 = VERTEX_POINT ( 'NONE', #5781 ) ;
#13631 = DIRECTION ( 'NONE',  ( 1.000000000000000000, 0.000000000000000000, 0.000000000000000000 ) ) ;
#13632 = VECTOR ( 'NONE', #15253, 1000.000000000000000 ) ;
#13633 = FACE_OUTER_BOUND ( 'NONE', #4998, .T. ) ;
#13634 = CIRCLE ( 'NONE', #12101, 2.649999999999992806 ) ;
#13635 = DIRECTION ( 'NONE',  ( -0.000000000000000000, 1.000000000000000000, 1.224646799147353207E-16 ) ) ;
#13636 = ORIENTED_EDGE ( 'NONE', *, *, #10063, .F. ) ;
#13637 = AXIS2_PLACEMENT_3D ( 'NONE', #2955, #100, #14381 ) ;
#13638 = FACE_OUTER_BOUND ( 'NONE', #3512, .T. ) ;
#13639 = PRODUCT_DEFINITION_SHAPE ( 'NONE', 'NONE',  #18823 ) ;
#13640 = LINE ( 'NONE', #5047, #1769 ) ;
#13641 = EDGE_LOOP ( 'NONE', ( #6081, #11874, #2780, #17868 ) ) ;
#13642 = EDGE_LOOP ( 'NONE', ( #3424, #17605, #3791, #13940 ) ) ;
#13643 = AXIS2_PLACEMENT_3D ( 'NONE', #15465, #9455, #18027 ) ;
#13644 = EDGE_CURVE ( 'NONE', #10933, #6918, #18633, .T. ) ;
#13645 = CIRCLE ( 'NONE', #3621, 12.00000000001200817 ) ;
#13646 = EDGE_CURVE ( 'NONE', #11202, #3100, #4730, .T. ) ;
#13647 = ORIENTED_EDGE ( 'NONE', *, *, #3039, .F. ) ;
#13648 = CIRCLE ( 'NONE', #9387, 12.00000000001200284 ) ;
#13649 =( REPRESENTATION_RELATIONSHIP ('NONE','NONE', #11014, #8256 ) REPRESENTATION_RELATIONSHIP_WITH_TRANSFORMATION ( #401 )SHAPE_REPRESENTATION_RELATIONSHIP( ) );
#13650 = ORIENTED_EDGE ( 'NONE', *, *, #2708, .T. ) ;
#13651 = DIRECTION ( 'NONE',  ( 0.000000000000000000, 0.000000000000000000, 1.000000000000000000 ) ) ;
#13652 = FACE_OUTER_BOUND ( 'NONE', #16161, .T. ) ;
#13653 = CARTESIAN_POINT ( 'NONE',  ( 0.000000000000000000, -33.71303790549234947, -53.22058882792234158 ) ) ;
#13654 = CARTESIAN_POINT ( 'NONE',  ( 5.000000000000000000, 53.22058882792246237, -33.71303790549217183 ) ) ;
#13655 = DIRECTION ( 'NONE',  ( 0.000000000000000000, -0.000000000000000000, -1.000000000000000000 ) ) ;
#13656 = VECTOR ( 'NONE', #9435, 1000.000000000000000 ) ;
#13657 = CARTESIAN_POINT ( 'NONE',  ( 2.500000000000000000, 1.768423874527825124, 1.020999999999998797 ) ) ;
#13658 = CARTESIAN_POINT ( 'NONE',  ( 0.000000000000000000, 55.51919907100666762, -9.823366686500051514 ) ) ;
#13659 = ORIENTED_EDGE ( 'NONE', *, *, #8422, .T. ) ;
#13660 = CARTESIAN_POINT ( 'NONE',  ( -5.032868406504333869, -28.36021363089093938, -2.000000000000000000 ) ) ;
#13661 = ORIENTED_EDGE ( 'NONE', *, *, #18062, .T. ) ;
#13662 = AXIS2_PLACEMENT_3D ( 'NONE', #862, #762, #18277 ) ;
#13663 = FACE_OUTER_BOUND ( 'NONE', #1067, .T. ) ;
#13664 = EDGE_CURVE ( 'NONE', #15213, #7351, #5946, .T. ) ;
#13665 = DIRECTION ( 'NONE',  ( 0.000000000000000000, 1.000000000000000000, 3.491481338843133355E-15 ) ) ;
#13666 = DIRECTION ( 'NONE',  ( 0.000000000000000000, 0.3090169943749411785, 0.9510565162951555296 ) ) ;
#13667 = ORIENTED_EDGE ( 'NONE', *, *, #11799, .T. ) ;
#13668 = ORIENTED_EDGE ( 'NONE', *, *, #10693, .T. ) ;
#13669 = CIRCLE ( 'NONE', #18531, 2.041999999999999815 ) ;
#13670 = PLANE ( 'NONE',  #6584 ) ;
#13671 = DIRECTION ( 'NONE',  ( 0.000000000000000000, 0.000000000000000000, 1.000000000000000000 ) ) ;
#13672 = DIRECTION ( 'NONE',  ( -1.000000000000000000, 0.000000000000000000, -0.000000000000000000 ) ) ;
#13673 = ORIENTED_EDGE ( 'NONE', *, *, #7230, .T. ) ;
#13674 = EDGE_CURVE ( 'NONE', #10426, #7667, #17805, .T. ) ;
#13675 = EDGE_CURVE ( 'NONE', #18365, #7876, #7295, .T. ) ;
#13676 = AXIS2_PLACEMENT_3D ( 'NONE', #16541, #3497, #3600 ) ;
#13677 = CARTESIAN_POINT ( 'NONE',  ( 0.000000000000000000, 0.000000000000000000, 0.000000000000000000 ) ) ;
#13678 = ADVANCED_FACE ( 'NONE', ( #11390, #14345, #15956, #13200, #18723, #9967, #2736 ), #14265, .T. ) ;
#13679 = DIRECTION ( 'NONE',  ( -1.000000000000000000, -0.000000000000000000, -0.000000000000000000 ) ) ;
#13680 = CYLINDRICAL_SURFACE ( 'NONE', #10567, 63.00000000006298961 ) ;
#13681 = EDGE_CURVE ( 'NONE', #1435, #2471, #17209, .T. ) ;
#13682 = ORIENTED_EDGE ( 'NONE', *, *, #10079, .T. ) ;
#13683 = DIRECTION ( 'NONE',  ( 1.000000000000000000, 0.000000000000000000, 0.000000000000000000 ) ) ;
#13684 = ORIENTED_EDGE ( 'NONE', *, *, #14352, .T. ) ;
#13685 = CYLINDRICAL_SURFACE ( 'NONE', #9066, 63.00000000006298961 ) ;
#13686 = EDGE_LOOP ( 'NONE', ( #2117, #4712, #3208, #8462 ) ) ;
#13687 = EDGE_CURVE ( 'NONE', #4094, #13520, #14467, .T. ) ;
#13688 = CARTESIAN_POINT ( 'NONE',  ( 2.449293598294706513E-15, -30.00000000000000000, -20.00000000000000000 ) ) ;
#13689 = CARTESIAN_POINT ( 'NONE',  ( -10.00000000000000000, 0.000000000000000000, 0.000000000000000000 ) ) ;
#13690 = ORIENTED_EDGE ( 'NONE', *, *, #2606, .T. ) ;
#13691 = VERTEX_POINT ( 'NONE', #1307 ) ;
#13692 = DIRECTION ( 'NONE',  ( -1.000000000000000000, 0.000000000000000000, -0.000000000000000000 ) ) ;
#13693 = AXIS2_PLACEMENT_3D ( 'NONE', #1739, #14694, #8796 ) ;
#13694 = SURFACE_SIDE_STYLE ('',( #5106 ) ) ;
#13695 = ORIENTED_EDGE ( 'NONE', *, *, #7945, .T. ) ;
#13696 = CARTESIAN_POINT ( 'NONE',  ( 13.90576474687299680, 10.00000000000000000, 42.79754323328179311 ) ) ;
#13697 = CARTESIAN_POINT ( 'NONE',  ( 3.436319922986518449, -2.634841920959471562, -3.531542292954761741 ) ) ;
#13698 = AXIS2_PLACEMENT_3D ( 'NONE', #14788, #1743, #17741 ) ;
#13699 = CARTESIAN_POINT ( 'NONE',  ( 0.000000000000000000, -17.25000000000000355, 0.000000000000000000 ) ) ;
#13700 = EDGE_CURVE ( 'NONE', #7777, #451, #5938, .T. ) ;
#13701 = VERTEX_POINT ( 'NONE', #7014 ) ;
#13702 = VECTOR ( 'NONE', #17169, 1000.000000000000000 ) ;
#13703 = VERTEX_POINT ( 'NONE', #12922 ) ;
#13704 = CARTESIAN_POINT ( 'NONE',  ( 3.453038570460273071, 2.625189405340834448, -3.535263753543585352 ) ) ;
#13705 = CARTESIAN_POINT ( 'NONE',  ( 5.000000000000000000, -48.50907078259351835, -40.19788616105663692 ) ) ;
#13706 = DIRECTION ( 'NONE',  ( 0.000000000000000000, 0.000000000000000000, 1.000000000000000000 ) ) ;
#13707 = ORIENTED_EDGE ( 'NONE', *, *, #5525, .F. ) ;
#13708 = DIRECTION ( 'NONE',  ( -1.000000000000000000, 0.000000000000000000, 0.000000000000000000 ) ) ;
#13709 = FACE_OUTER_BOUND ( 'NONE', #5158, .T. ) ;
#13710 = LINE ( 'NONE', #7690, #3733 ) ;
#13711 = DIRECTION ( 'NONE',  ( -1.000000000000000000, -0.000000000000000000, -0.000000000000000000 ) ) ;
#13712 = VERTEX_POINT ( 'NONE', #4264 ) ;
#13713 = FACE_OUTER_BOUND ( 'NONE', #7746, .T. ) ;
#13714 = ORIENTED_EDGE ( 'NONE', *, *, #1469, .T. ) ;
#13715 = CARTESIAN_POINT ( 'NONE',  ( 10.00000000000000000, -53.89344778774823652, 16.10733642026462675 ) ) ;
#13716 = CARTESIAN_POINT ( 'NONE',  ( 10.00000000000000000, 55.51919907100666762, -9.823366686500051514 ) ) ;
#13717 = AXIS2_PLACEMENT_3D ( 'NONE', #1222, #5687, #11301 ) ;
#13718 = EDGE_CURVE ( 'NONE', #5558, #5435, #8978, .T. ) ;
#13719 = ORIENTED_EDGE ( 'NONE', *, *, #6693, .F. ) ;
#13720 = ORIENTED_EDGE ( 'NONE', *, *, #18022, .T. ) ;
#13721 = CARTESIAN_POINT ( 'NONE',  ( -26.29305231718568336, -26.50000000000000000, -19.10302069950552095 ) ) ;
#13722 = CARTESIAN_POINT ( 'NONE',  ( 4.000000000000000000, -1.700175430507292473, -3.320327275037661785 ) ) ;
#13723 = CARTESIAN_POINT ( 'NONE',  ( -117.1020693116508085, -30.00000000000000000, 17.04080595179778967 ) ) ;
#13724 = DIRECTION ( 'NONE',  ( 0.000000000000000000, 0.000000000000000000, 1.000000000000000000 ) ) ;
#13725 = AXIS2_PLACEMENT_3D ( 'NONE', #6431, #9383, #6720 ) ;
#13726 = FACE_OUTER_BOUND ( 'NONE', #13641, .T. ) ;
#13727 = DIRECTION ( 'NONE',  ( -0.000000000000000000, -0.000000000000000000, 1.000000000000000000 ) ) ;
#13728 = ORIENTED_EDGE ( 'NONE', *, *, #405, .F. ) ;
#13729 = DIRECTION ( 'NONE',  ( -0.000000000000000000, 1.000000000000000000, -0.000000000000000000 ) ) ;
#13730 =( LENGTH_UNIT ( ) NAMED_UNIT ( * ) SI_UNIT ( .MILLI., .METRE. ) );
#13731 = LINE ( 'NONE', #16869, #13023 ) ;
#13732 = ORIENTED_EDGE ( 'NONE', *, *, #16329, .T. ) ;
#13733 = EDGE_CURVE ( 'NONE', #1152, #9197, #471, .T. ) ;
#13734 = ORIENTED_EDGE ( 'NONE', *, *, #17359, .T. ) ;
#13735 = CIRCLE ( 'NONE', #14314, 2.649999999999999467 ) ;
#13736 = ADVANCED_FACE ( 'NONE', ( #15103 ), #16526, .T. ) ;
#13737 = ORIENTED_EDGE ( 'NONE', *, *, #2199, .F. ) ;
#13738 = ORIENTED_EDGE ( 'NONE', *, *, #17158, .T. ) ;
#13740 = DIRECTION ( 'NONE',  ( 0.000000000000000000, 0.000000000000000000, 1.000000000000000000 ) ) ;
#13739 = VECTOR ( 'NONE', #15351, 1000.000000000000000 ) ;
#13741 = DIRECTION ( 'NONE',  ( -1.000000000000000000, -0.000000000000000000, -0.000000000000000000 ) ) ;
#13742 = CYLINDRICAL_SURFACE ( 'NONE', #16008, 26.24900000002624978 ) ;
#13743 = FILL_AREA_STYLE_COLOUR ( '', #6688 ) ;
#13744 = CARTESIAN_POINT ( 'NONE',  ( -10.00000000000000000, 42.79754323328179311, -11.25576474687299644 ) ) ;
#13745 = DIRECTION ( 'NONE',  ( 0.000000000000000000, 0.000000000000000000, -1.000000000000000000 ) ) ;
#13746 = FACE_OUTER_BOUND ( 'NONE', #356, .T. ) ;
#13747 = EDGE_LOOP ( 'NONE', ( #2180, #12333, #3973, #9193 ) ) ;
#13748 = DIRECTION ( 'NONE',  ( 1.000000000000000000, 0.000000000000000000, 0.000000000000000000 ) ) ;
#13749 = EDGE_LOOP ( 'NONE', ( #16757, #14009 ) ) ;
#13750 = FACE_OUTER_BOUND ( 'NONE', #2293, .T. ) ;
#13751 = CARTESIAN_POINT ( 'NONE',  ( 10.00000000000000000, -16.10733642026522006, 53.89344778774807310 ) ) ;
#13752 = ORIENTED_EDGE ( 'NONE', *, *, #10628, .T. ) ;
#13753 = VERTEX_POINT ( 'NONE', #8991 ) ;
#13754 = PLANE ( 'NONE',  #1404 ) ;
#13755 = DIRECTION ( 'NONE',  ( 0.000000000000000000, 1.000000000000000000, 0.000000000000000000 ) ) ;
#13756 = TOROIDAL_SURFACE ( 'NONE', #2495, 2.700000000000000622, 0.2000000000000000111 ) ;
#13757 = DIRECTION ( 'NONE',  ( 0.000000000000000000, 0.000000000000000000, 1.000000000000000000 ) ) ;
#13758 = ORIENTED_EDGE ( 'NONE', *, *, #4067, .F. ) ;
#13759 = CYLINDRICAL_SURFACE ( 'NONE', #5948, 2.649999999999992806 ) ;
#13760 = PLANE ( 'NONE',  #18253 ) ;
#13761 = CARTESIAN_POINT ( 'NONE',  ( 0.000000000000000000, -24.97244012287543669, 57.83923611457311154 ) ) ;
#13762 = ORIENTED_EDGE ( 'NONE', *, *, #7962, .F. ) ;
#13763 = DIRECTION ( 'NONE',  ( -1.000000000000000000, -0.000000000000000000, -0.000000000000000000 ) ) ;
#13764 = AXIS2_PLACEMENT_3D ( 'NONE', #13335, #3231, #11622 ) ;
#13765 = ORIENTED_EDGE ( 'NONE', *, *, #2610, .T. ) ;
#13766 = UNCERTAINTY_MEASURE_WITH_UNIT (LENGTH_MEASURE( 1.000000000000000082E-05 ), #486, 'distance_accuracy_value', 'NONE');
#13767 = DIRECTION ( 'NONE',  ( -1.000000000000000000, -0.000000000000000000, 0.000000000000000000 ) ) ;
#13768 = ORIENTED_EDGE ( 'NONE', *, *, #14064, .T. ) ;
#13769 = ADVANCED_FACE ( 'NONE', ( #1947, #13487 ), #9184, .F. ) ;
#13770 = EDGE_CURVE ( 'NONE', #6237, #10072, #175, .T. ) ;
#13771 = ADVANCED_FACE ( 'NONE', ( #4814 ), #4904, .T. ) ;
#13772 = CARTESIAN_POINT ( 'NONE',  ( 0.000000000000000000, -18.64666490672335186, -53.06836994729252410 ) ) ;
#13773 = CARTESIAN_POINT ( 'NONE',  ( 0.1750025118121568690, 4.719839900820621104, -3.469254087858248070 ) ) ;
#13774 = ORIENTED_EDGE ( 'NONE', *, *, #14142, .F. ) ;
#13775 = ORIENTED_EDGE ( 'NONE', *, *, #17061, .T. ) ;
#13776 = DIRECTION ( 'NONE',  ( -1.000000000000000000, 0.000000000000000000, 0.000000000000000000 ) ) ;
#13777 = ADVANCED_FACE ( 'NONE', ( #10343 ), #10618, .T. ) ;
#13778 = EDGE_LOOP ( 'NONE', ( #11315, #17062, #5424, #16246 ) ) ;
#13779 = CYLINDRICAL_SURFACE ( 'NONE', #918, 63.00000000006298961 ) ;
#13780 = CIRCLE ( 'NONE', #7688, 33.00000000003299760 ) ;
#13781 = DIRECTION ( 'NONE',  ( 2.220446049250313081E-16, -0.000000000000000000, -1.000000000000000000 ) ) ;
#13782 = ADVANCED_FACE ( 'NONE', ( #11952 ), #8904, .F. ) ;
#13783 = DIRECTION ( 'NONE',  ( -1.000000000000000000, -0.000000000000000000, -0.000000000000000000 ) ) ;
#13784 = ORIENTED_EDGE ( 'NONE', *, *, #3429, .T. ) ;
#13785 = ORIENTED_EDGE ( 'NONE', *, *, #1538, .T. ) ;
#13786 = DIRECTION ( 'NONE',  ( 0.000000000000000000, 0.000000000000000000, -1.000000000000000000 ) ) ;
#13787 = CARTESIAN_POINT ( 'NONE',  ( 10.00000000000000000, -12.18267823974769293, 25.42247726998010648 ) ) ;
#13788 = LINE ( 'NONE', #15313, #537 ) ;
#13789 = VERTEX_POINT ( 'NONE', #14716 ) ;
#13790 = DIRECTION ( 'NONE',  ( -0.000000000000000000, 1.000000000000000000, -0.000000000000000000 ) ) ;
#13791 = EDGE_CURVE ( 'NONE', #5783, #15756, #8387, .T. ) ;
#13792 = AXIS2_PLACEMENT_3D ( 'NONE', #15267, #3953, #9651 ) ;
#13793 = DIRECTION ( 'NONE',  ( -1.000000000000000000, 0.000000000000000000, -0.000000000000000000 ) ) ;
#13794 = DIRECTION ( 'NONE',  ( -1.000000000000000000, -0.000000000000000000, 0.000000000000000000 ) ) ;
#13795 = VERTEX_POINT ( 'NONE', #1762 ) ;
#13796 = CARTESIAN_POINT ( 'NONE',  ( 10.00000000000000000, -57.83923611457338154, 24.97244012287480430 ) ) ;
#13797 = VERTEX_POINT ( 'NONE', #13579 ) ;
#13798 = CARTESIAN_POINT ( 'NONE',  ( 10.00000000000000000, 25.42247726998014912, 12.18267823974760411 ) ) ;
#13799 = EDGE_LOOP ( 'NONE', ( #8051, #5951, #12109, #16086 ) ) ;
#13800 = DIRECTION ( 'NONE',  ( -0.000000000000000000, 1.000000000000000000, -0.000000000000000000 ) ) ;
#13801 = DIRECTION ( 'NONE',  ( -1.000000000000000000, 0.000000000000000000, 0.000000000000000000 ) ) ;
#13802 = EDGE_CURVE ( 'NONE', #12684, #11971, #16243, .T. ) ;
#13803 = MECHANICAL_DESIGN_GEOMETRIC_PRESENTATION_REPRESENTATION (  '', ( #14714 ), #2246 ) ;
#13804 = VERTEX_POINT ( 'NONE', #3197 ) ;
#13805 = ORIENTED_EDGE ( 'NONE', *, *, #10156, .T. ) ;
#13806 = CARTESIAN_POINT ( 'NONE',  ( -90.67999921423555065, 1.821459649775647449E-14, -4.751589320297106234 ) ) ;
#13807 = CARTESIAN_POINT ( 'NONE',  ( 10.00000000000000000, -53.89344778774800915, -16.10733642026540480 ) ) ;
#13808 = CARTESIAN_POINT ( 'NONE',  ( 0.000000000000000000, 49.49802920186223076, 26.71881558261748069 ) ) ;
#13809 = DIRECTION ( 'NONE',  ( 1.000000000000000000, 0.000000000000000000, 0.000000000000000000 ) ) ;
#13810 = FACE_OUTER_BOUND ( 'NONE', #4873, .T. ) ;
#13811 = LINE ( 'NONE', #5043, #11125 ) ;
#13812 = ORIENTED_EDGE ( 'NONE', *, *, #12257, .T. ) ;
#13813 = CARTESIAN_POINT ( 'NONE',  ( -3.540020015735593439, -2.810662092924100630, -3.602146406945814672 ) ) ;
#13814 = CARTESIAN_POINT ( 'NONE',  ( 0.000000000000000000, 26.45033635316149301, 39.05576474687247668 ) ) ;
#13815 = ORIENTED_EDGE ( 'NONE', *, *, #10399, .F. ) ;
#13816 = EDGE_CURVE ( 'NONE', #7434, #9997, #3387, .T. ) ;
#13817 = CONTEXT_DEPENDENT_SHAPE_REPRESENTATION ( #15953, #3130 ) ;
#13818 = VERTEX_POINT ( 'NONE', #6338 ) ;
#13819 = ORIENTED_EDGE ( 'NONE', *, *, #2087, .T. ) ;
#13820 = VERTEX_POINT ( 'NONE', #4710 ) ;
#13821 = AXIS2_PLACEMENT_3D ( 'NONE', #4804, #2135, #3575 ) ;
#13822 = LINE ( 'NONE', #18109, #5377 ) ;
#13823 = LINE ( 'NONE', #4883, #30 ) ;
#13824 =( NAMED_UNIT ( * ) PLANE_ANGLE_UNIT ( ) SI_UNIT ( $, .RADIAN. ) );
#13825 = AXIS2_PLACEMENT_3D ( 'NONE', #13275, #15689, #4518 ) ;
#13826 = FACE_OUTER_BOUND ( 'NONE', #15241, .T. ) ;
#13827 = EDGE_CURVE ( 'NONE', #12049, #3333, #17953, .T. ) ;
#13828 = CARTESIAN_POINT ( 'NONE',  ( 10.00000000000000000, -23.24033432160398505, -58.55669782892484676 ) ) ;
#13829 = LINE ( 'NONE', #9452, #13739 ) ;
#13830 = LINE ( 'NONE', #12409, #15071 ) ;
#13831 = ORIENTED_EDGE ( 'NONE', *, *, #4023, .F. ) ;
#13832 = DIRECTION ( 'NONE',  ( 0.000000000000000000, 0.000000000000000000, 1.000000000000000000 ) ) ;
#13833 = EDGE_LOOP ( 'NONE', ( #18166, #15955, #7764, #13714 ) ) ;
#13834 = EDGE_CURVE ( 'NONE', #3113, #2015, #13550, .T. ) ;
#13835 = CYLINDRICAL_SURFACE ( 'NONE', #13792, 24.00000000002400213 ) ;
#13836 = DIRECTION ( 'NONE',  ( 1.000000000000000000, 0.000000000000000000, 0.000000000000000000 ) ) ;
#13837 = ORIENTED_EDGE ( 'NONE', *, *, #7263, .T. ) ;
#13838 = ORIENTED_EDGE ( 'NONE', *, *, #1664, .T. ) ;
#13839 = CARTESIAN_POINT ( 'NONE',  ( -10.00000000000000000, 0.000000000000000000, 0.000000000000000000 ) ) ;
#13840 = DIRECTION ( 'NONE',  ( 0.9820818503191364179, 7.285838599102589797E-17, -0.1884548733085492089 ) ) ;
#13841 = PRODUCT_DEFINITION_FORMATION_WITH_SPECIFIED_SOURCE ( 'ANY', '', #3293, .NOT_KNOWN. ) ;
#13842 = DIRECTION ( 'NONE',  ( -0.000000000000000000, 1.000000000000000000, 0.000000000000000000 ) ) ;
#13843 = ORIENTED_EDGE ( 'NONE', *, *, #14480, .T. ) ;
#13844 = AXIS2_PLACEMENT_3D ( 'NONE', #9580, #1025, #16929 ) ;
#13845 = DIRECTION ( 'NONE',  ( -1.000000000000000000, 0.000000000000000000, 0.000000000000000000 ) ) ;
#13846 = CYLINDRICAL_SURFACE ( 'NONE', #5482, 25.00000000000000000 ) ;
#13847 = AXIS2_PLACEMENT_3D ( 'NONE', #13798, #18465, #5517 ) ;
#13848 = DIRECTION ( 'NONE',  ( -1.000000000000000000, 0.000000000000000000, 0.000000000000000000 ) ) ;
#13849 = ORIENTED_EDGE ( 'NONE', *, *, #9153, .F. ) ;
#13850 = CARTESIAN_POINT ( 'NONE',  ( 0.000000000000000000, 3.000000000000000000, -150.0000000000000000 ) ) ;
#13851 = VECTOR ( 'NONE', #1666, 1000.000000000000227 ) ;
#13852 = VERTEX_POINT ( 'NONE', #17674 ) ;
#13853 = CYLINDRICAL_SURFACE ( 'NONE', #8751, 2.649999999999999467 ) ;
#13854 = AXIS2_PLACEMENT_3D ( 'NONE', #8408, #11164, #16995 ) ;
#13855 = EDGE_LOOP ( 'NONE', ( #14879, #218, #1814, #8323 ) ) ;
#13856 = DIRECTION ( 'NONE',  ( -1.000000000000000000, -0.000000000000000000, -0.000000000000000000 ) ) ;
#13857 = DIRECTION ( 'NONE',  ( 0.000000000000000000, 0.000000000000000000, 1.000000000000000000 ) ) ;
#13858 = CARTESIAN_POINT ( 'NONE',  ( 10.00000000000000000, -10.11537145609416122, 55.33199130079781014 ) ) ;
#13859 = ORIENTED_EDGE ( 'NONE', *, *, #889, .T. ) ;
#13860 = VERTEX_POINT ( 'NONE', #10428 ) ;
#13861 = DIRECTION ( 'NONE',  ( 0.000000000000000000, 1.000000000000000000, 0.000000000000000000 ) ) ;
#13862 =( NAMED_UNIT ( * ) SI_UNIT ( $, .STERADIAN. ) SOLID_ANGLE_UNIT ( ) );
#13863 = ORIENTED_EDGE ( 'NONE', *, *, #9443, .T. ) ;
#13864 = CARTESIAN_POINT ( 'NONE',  ( 10.00000000000000000, 55.51919907100653973, 9.823366686500859757 ) ) ;
#13865 = VECTOR ( 'NONE', #7589, 1000.000000000000000 ) ;
#13866 = AXIS2_PLACEMENT_3D ( 'NONE', #18030, #18381, #5335 ) ;
#13867 = AXIS2_PLACEMENT_3D ( 'NONE', #2300, #5163, #6497 ) ;
#13868 = CIRCLE ( 'NONE', #2616, 63.00000000006298961 ) ;
#13869 = CIRCLE ( 'NONE', #16307, 2.649999999999992806 ) ;
#13870 = VECTOR ( 'NONE', #5989, 1000.000000000000000 ) ;
#13871 = EDGE_CURVE ( 'NONE', #6780, #17410, #5330, .T. ) ;
#13872 = DIRECTION ( 'NONE',  ( -1.000000000000000000, -0.000000000000000000, 0.000000000000000000 ) ) ;
#13873 = ADVANCED_FACE ( 'NONE', ( #14915 ), #16341, .T. ) ;
#13874 = DIRECTION ( 'NONE',  ( 0.9938152567191714803, 0.000000000000000000, -0.1110460963393456596 ) ) ;
#13875 = ORIENTED_EDGE ( 'NONE', *, *, #2708, .F. ) ;
#13876 = DIRECTION ( 'NONE',  ( 1.000000000000000000, 0.000000000000000000, 0.000000000000000000 ) ) ;
#13877 = EDGE_CURVE ( 'NONE', #18371, #7713, #11183, .T. ) ;
#13878 = VECTOR ( 'NONE', #16330, 1000.000000000000000 ) ;
#13879 = ORIENTED_EDGE ( 'NONE', *, *, #4834, .F. ) ;
#13880 = CARTESIAN_POINT ( 'NONE',  ( 0.000000000000000000, 13.24999999999999467, 0.000000000000000000 ) ) ;
#13881 = CARTESIAN_POINT ( 'NONE',  ( 3.061616997868383043E-15, 11.24999999999999645, -25.00000000000000000 ) ) ;
#13883 = AXIS2_PLACEMENT_3D ( 'NONE', #8937, #10188, #3055 ) ;
#13882 = CARTESIAN_POINT ( 'NONE',  ( 10.00000000000000000, -1.335003989222025123, 56.23315539212689629 ) ) ;
#13884 = ORIENTED_EDGE ( 'NONE', *, *, #4028, .F. ) ;
#13885 = DIRECTION ( 'NONE',  ( -0.000000000000000000, -0.000000000000000000, 1.000000000000000000 ) ) ;
#13886 = VERTEX_POINT ( 'NONE', #14133 ) ;
#13887 = ADVANCED_FACE ( 'NONE', ( #15280 ), #1097, .T. ) ;
#13888 = VECTOR ( 'NONE', #12572, 1000.000000000000000 ) ;
#13889 = CARTESIAN_POINT ( 'NONE',  ( 0.000000000000000000, -42.79754323328189969, -16.55576474687263300 ) ) ;
#13890 = CARTESIAN_POINT ( 'NONE',  ( 0.000000000000000000, 0.000000000000000000, 0.000000000000000000 ) ) ;
#13891 = CIRCLE ( 'NONE', #10542, 24.00000000002400213 ) ;
#13892 = ORIENTED_EDGE ( 'NONE', *, *, #4202, .F. ) ;
#13893 = VERTEX_POINT ( 'NONE', #13954 ) ;
#13894 = TOROIDAL_SURFACE ( 'NONE', #2036, 5.384454397937118664, 0.5155456020628804703 ) ;
#13895 = CARTESIAN_POINT ( 'NONE',  ( 0.000000000000000000, 0.000000000000000000, 0.000000000000000000 ) ) ;
#13897 = EDGE_CURVE ( 'NONE', #5831, #13703, #17504, .T. ) ;
#13896 = EDGE_LOOP ( 'NONE', ( #2533, #18590, #1204, #6224 ) ) ;
#13898 = DIRECTION ( 'NONE',  ( -1.000000000000000000, 0.000000000000000000, 0.000000000000000000 ) ) ;
#13899 = CARTESIAN_POINT ( 'NONE',  ( 0.000000000000000000, 57.83923611457355918, -24.97244012287440285 ) ) ;
#13900 =( REPRESENTATION_RELATIONSHIP ('NONE','NONE', #11014, #2386 ) REPRESENTATION_RELATIONSHIP_WITH_TRANSFORMATION ( #10764 )SHAPE_REPRESENTATION_RELATIONSHIP( ) );
#13901 = AXIS2_PLACEMENT_3D ( 'NONE', #18372, #12281, #18282 ) ;
#13902 = ADVANCED_FACE ( 'NONE', ( #919 ), #18326, .T. ) ;
#13903 = AXIS2_PLACEMENT_3D ( 'NONE', #4863, #6577, #12382 ) ;
#13904 = ADVANCED_FACE ( 'NONE', ( #2229 ), #8243, .T. ) ;
#13905 = CIRCLE ( 'NONE', #17858, 24.00000000002399503 ) ;
#13906 = AXIS2_PLACEMENT_3D ( 'NONE', #10227, #11395, #8886 ) ;
#13907 = VERTEX_POINT ( 'NONE', #9760 ) ;
#13908 = EDGE_CURVE ( 'NONE', #7103, #4060, #4746, .T. ) ;
#13909 = ORIENTED_EDGE ( 'NONE', *, *, #10628, .F. ) ;
#13910 = CARTESIAN_POINT ( 'NONE',  ( 10.00000000000000000, -49.49802920186242972, 26.71881558261712186 ) ) ;
#13911 = CARTESIAN_POINT ( 'NONE',  ( 4.000000000000000000, -1.942223658245635809, -0.3516579909967643691 ) ) ;
#13913 = EDGE_CURVE ( 'NONE', #9460, #538, #15394, .T. ) ;
#13912 = FACE_OUTER_BOUND ( 'NONE', #13243, .T. ) ;
#13914 = CARTESIAN_POINT ( 'NONE',  ( 0.000000000000000000, 0.000000000000000000, 0.000000000000000000 ) ) ;
#13915 = LINE ( 'NONE', #6764, #9070 ) ;
#13916 = CIRCLE ( 'NONE', #12088, 24.00000000002400213 ) ;
#13917 = CARTESIAN_POINT ( 'NONE',  ( 0.000000000000000000, 0.000000000000000000, 0.000000000000000000 ) ) ;
#13918 = ORIENTED_EDGE ( 'NONE', *, *, #15050, .F. ) ;
#13919 = CARTESIAN_POINT ( 'NONE',  ( -90.72413394419160682, -14.11572627500821042, 4.947285117213267469 ) ) ;
#13920 = VECTOR ( 'NONE', #6372, 1000.000000000000000 ) ;
#13921 = CARTESIAN_POINT ( 'NONE',  ( 0.000000000000000000, 5.086963483077590276, -27.72801475327276677 ) ) ;
#13922 = CARTESIAN_POINT ( 'NONE',  ( 10.00000000000000000, -25.42247726998005675, -12.18267823974779240 ) ) ;
#13923 = CIRCLE ( 'NONE', #15129, 24.00000000002399858 ) ;
#13924 = AXIS2_PLACEMENT_3D ( 'NONE', #12982, #10118, #208 ) ;
#13925 = ORIENTED_EDGE ( 'NONE', *, *, #16227, .T. ) ;
#13926 = ORIENTED_EDGE ( 'NONE', *, *, #9491, .F. ) ;
#13927 = AXIS2_PLACEMENT_3D ( 'NONE', #11506, #7025, #17322 ) ;
#13928 = VERTEX_POINT ( 'NONE', #3857 ) ;
#13929 = AXIS2_PLACEMENT_3D ( 'NONE', #8026, #4979, #18315 ) ;
#13930 = DIRECTION ( 'NONE',  ( -0.000000000000000000, 1.000000000000000000, -0.000000000000000000 ) ) ;
#13931 = CARTESIAN_POINT ( 'NONE',  ( 10.00000000000000000, -40.58063702438372644, 39.14194549634347453 ) ) ;
#13932 = AXIS2_PLACEMENT_3D ( 'NONE', #10409, #2025, #14695 ) ;
#13933 = AXIS2_PLACEMENT_3D ( 'NONE', #2105, #1719, #9329 ) ;
#13934 = EDGE_CURVE ( 'NONE', #16268, #8822, #6717, .T. ) ;
#13935 = CARTESIAN_POINT ( 'NONE',  ( -85.22968676783801811, 1.000000000000018208, -0.5330212624288650503 ) ) ;
#13936 = DIRECTION ( 'NONE',  ( -1.000000000000000000, -0.000000000000000000, -0.000000000000000000 ) ) ;
#13937 = DIRECTION ( 'NONE',  ( 0.000000000000000000, 1.000000000000000000, 0.000000000000000000 ) ) ;
#13938 = DIRECTION ( 'NONE',  ( 0.000000000000000000, -1.000000000000000000, 0.000000000000000000 ) ) ;
#13939 = DIRECTION ( 'NONE',  ( 0.000000000000000000, 0.000000000000000000, -1.000000000000000000 ) ) ;
#13940 = ORIENTED_EDGE ( 'NONE', *, *, #5768, .T. ) ;
#13941 = CARTESIAN_POINT ( 'NONE',  ( -2.354826896168714434, -6.962563485461402024, -1.000000000000000000 ) ) ;
#13942 = EDGE_LOOP ( 'NONE', ( #5910, #7491, #7820, #2492 ) ) ;
#13943 = DIRECTION ( 'NONE',  ( -1.000000000000000000, 0.000000000000000000, 0.000000000000000000 ) ) ;
#13944 = CARTESIAN_POINT ( 'NONE',  ( 0.000000000000000000, 0.000000000000000000, 0.000000000000000000 ) ) ;
#13945 = ORIENTED_EDGE ( 'NONE', *, *, #13500, .T. ) ;
#13946 = ORIENTED_EDGE ( 'NONE', *, *, #4807, .F. ) ;
#13947 = FACE_OUTER_BOUND ( 'NONE', #5839, .T. ) ;
#13948 = DIRECTION ( 'NONE',  ( 0.3090169943749581649, 6.123233995736766036E-17, -0.9510565162951500895 ) ) ;
#13949 = CIRCLE ( 'NONE', #18194, 12.00000000001200462 ) ;
#13950 = DIRECTION ( 'NONE',  ( 0.000000000000000000, -0.000000000000000000, 1.000000000000000000 ) ) ;
#13951 = ORIENTED_EDGE ( 'NONE', *, *, #17403, .F. ) ;
#13952 = AXIS2_PLACEMENT_3D ( 'NONE', #6784, #5461, #3557 ) ;
#13953 = AXIS2_PLACEMENT_3D ( 'NONE', #2193, #6677, #11244 ) ;
#13954 = CARTESIAN_POINT ( 'NONE',  ( 10.00000000000000000, 40.70683587898012235, -38.81885513159945589 ) ) ;
#13955 = LINE ( 'NONE', #10705, #7599 ) ;
#13956 = FACE_OUTER_BOUND ( 'NONE', #17025, .T. ) ;
#13957 = EDGE_CURVE ( 'NONE', #17358, #7974, #3762, .T. ) ;
#13958 = CARTESIAN_POINT ( 'NONE',  ( -1.128893538851230005, 13.24999999999999467, 23.47286943213250154 ) ) ;
#13959 = AXIS2_PLACEMENT_3D ( 'NONE', #9222, #6559, #2270 ) ;
#13960 = AXIS2_PLACEMENT_3D ( 'NONE', #4617, #10425, #5942 ) ;
#13961 = AXIS2_PLACEMENT_3D ( 'NONE', #6189, #11907, #17807 ) ;
#13962 = EDGE_LOOP ( 'NONE', ( #4835, #12585, #628, #1467 ) ) ;
#13963 = UNCERTAINTY_MEASURE_WITH_UNIT (LENGTH_MEASURE( 1.000000000000000082E-05 ), #4785, 'distance_accuracy_value', 'NONE');
#13964 = DIRECTION ( 'NONE',  ( 0.000000000000000000, 0.000000000000000000, 1.000000000000000000 ) ) ;
#13965 = EDGE_LOOP ( 'NONE', ( #5032, #1679, #7568, #5079, #250 ) ) ;
#13966 = DIRECTION ( 'NONE',  ( 1.000000000000000000, -0.000000000000000000, -0.000000000000000000 ) ) ;
#13967 = DIRECTION ( 'NONE',  ( 0.000000000000000000, 0.000000000000000000, -1.000000000000000000 ) ) ;
#13968 = LINE ( 'NONE', #13858, #2741 ) ;
#13969 = ORIENTED_EDGE ( 'NONE', *, *, #17820, .F. ) ;
#13970 = EDGE_LOOP ( 'NONE', ( #4016, #7094, #12085, #6773, #14843, #9425 ) ) ;
#13971 = DIRECTION ( 'NONE',  ( -1.000000000000000000, -0.000000000000000000, 0.000000000000000000 ) ) ;
#13972 = FILL_AREA_STYLE ('',( #8258 ) ) ;
#13973 = VERTEX_POINT ( 'NONE', #9555 ) ;
#13974 = DIRECTION ( 'NONE',  ( 0.000000000000000000, 0.000000000000000000, 1.000000000000000000 ) ) ;
#13975 = EDGE_CURVE ( 'NONE', #1379, #8411, #11124, .T. ) ;
#13976 = AXIS2_PLACEMENT_3D ( 'NONE', #5314, #16952, #3998 ) ;
#13977 = ADVANCED_FACE ( 'NONE', ( #6804 ), #13759, .F. ) ;
#13978 = CARTESIAN_POINT ( 'NONE',  ( 10.04305231718605285, -30.00000000000000000, -30.90933677959240811 ) ) ;
#13979 = FACE_OUTER_BOUND ( 'NONE', #14308, .T. ) ;
#13980 = ORIENTED_EDGE ( 'NONE', *, *, #18676, .T. ) ;
#13981 = CARTESIAN_POINT ( 'NONE',  ( 0.000000000000000000, 2.357898499370432166, -2.385244779468109755E-15 ) ) ;
#13982 = ORIENTED_EDGE ( 'NONE', *, *, #7624, .F. ) ;
#13983 = CARTESIAN_POINT ( 'NONE',  ( 0.000000000000000000, -50.71018745830461683, 24.33982105418882469 ) ) ;
#13984 = CARTESIAN_POINT ( 'NONE',  ( 4.999999999999999112, 62.72529079327815538, -5.876895005581753928 ) ) ;
#13985 = CARTESIAN_POINT ( 'NONE',  ( 11.14999999999999680, 0.000000000000000000, 0.000000000000000000 ) ) ;
#13986 = EDGE_LOOP ( 'NONE', ( #11190, #12979 ) ) ;
#13987 = DIRECTION ( 'NONE',  ( 1.000000000000000000, -0.000000000000000000, -0.000000000000000000 ) ) ;
#13988 = ORIENTED_EDGE ( 'NONE', *, *, #16561, .T. ) ;
#13989 = AXIS2_PLACEMENT_3D ( 'NONE', #13864, #12063, #10812 ) ;
#13990 = CARTESIAN_POINT ( 'NONE',  ( 0.000000000000000000, 49.49802920186260735, -26.71881558261677370 ) ) ;
#13991 = FACE_OUTER_BOUND ( 'NONE', #14170, .T. ) ;
#13992 = ORIENTED_EDGE ( 'NONE', *, *, #12161, .T. ) ;
#13993 = ORIENTED_EDGE ( 'NONE', *, *, #1827, .T. ) ;
#13994 =( NAMED_UNIT ( * ) SI_UNIT ( $, .STERADIAN. ) SOLID_ANGLE_UNIT ( ) );
#13995 = EDGE_CURVE ( 'NONE', #10460, #6241, #2933, .T. ) ;
#13996 = ORIENTED_EDGE ( 'NONE', *, *, #2849, .T. ) ;
#13997 = CARTESIAN_POINT ( 'NONE',  ( -0.3789929286210603765, 11.24999999999999645, 24.99712712213256438 ) ) ;
#13998 = CARTESIAN_POINT ( 'NONE',  ( -12.69999999999999929, 0.000000000000000000, -27.00000000000000355 ) ) ;
#13999 = AXIS2_PLACEMENT_3D ( 'NONE', #463, #11291, #17113 ) ;
#14000 = CIRCLE ( 'NONE', #4275, 2.649999999999992806 ) ;
#14001 = EDGE_LOOP ( 'NONE', ( #12030, #7670, #9550, #703 ) ) ;
#14002 = ORIENTED_EDGE ( 'NONE', *, *, #15758, .F. ) ;
#14003 = CARTESIAN_POINT ( 'NONE',  ( 0.000000000000000000, -30.00000000000000000, 0.000000000000000000 ) ) ;
#14004 = FACE_BOUND ( 'NONE', #4362, .T. ) ;
#14005 = CARTESIAN_POINT ( 'NONE',  ( 0.000000000000000000, 0.000000000000000000, 0.000000000000000000 ) ) ;
#14006 = DIRECTION ( 'NONE',  ( 0.000000000000000000, 0.000000000000000000, 1.000000000000000000 ) ) ;
#14007 = FACE_OUTER_BOUND ( 'NONE', #953, .T. ) ;
#14008 = FACE_OUTER_BOUND ( 'NONE', #3386, .T. ) ;
#14009 = ORIENTED_EDGE ( 'NONE', *, *, #2362, .T. ) ;
#14010 = DIRECTION ( 'NONE',  ( 0.000000000000000000, 0.000000000000000000, 1.000000000000000000 ) ) ;
#14011 = EDGE_CURVE ( 'NONE', #17219, #11928, #10522, .T. ) ;
#14012 = EDGE_CURVE ( 'NONE', #10666, #4042, #1995, .T. ) ;
#14013 = CARTESIAN_POINT ( 'NONE',  ( 2.500000000000000000, 2.629050547790028946E-15, 2.042000000000000259 ) ) ;
#14014 = EDGE_CURVE ( 'NONE', #2916, #5427, #2518, .T. ) ;
#14015 = DIRECTION ( 'NONE',  ( 0.000000000000000000, -0.9876883405951393247, 0.1564344650402205439 ) ) ;
#14016 = CARTESIAN_POINT ( 'NONE',  ( 10.00000000000000000, 1.017308535513159695, -56.37237871411032586 ) ) ;
#14017 = ADVANCED_FACE ( 'NONE', ( #10896 ), #2325, .T. ) ;
#14018 = EDGE_LOOP ( 'NONE', ( #12133, #6976 ) ) ;
#14019 = EDGE_CURVE ( 'NONE', #5875, #15951, #6271, .T. ) ;
#14020 = ORIENTED_EDGE ( 'NONE', *, *, #13532, .F. ) ;
#14021 = EDGE_CURVE ( 'NONE', #8500, #9007, #17822, .T. ) ;
#14022 = ORIENTED_EDGE ( 'NONE', *, *, #13194, .F. ) ;
#14023 = AXIS2_PLACEMENT_3D ( 'NONE', #3064, #5909, #8858 ) ;
#14024 = EDGE_CURVE ( 'NONE', #1826, #15974, #807, .T. ) ;
#14025 = DIRECTION ( 'NONE',  ( 0.000000000000000000, 0.000000000000000000, 1.000000000000000000 ) ) ;
#14026 = CYLINDRICAL_SURFACE ( 'NONE', #9759, 24.00000000002400213 ) ;
#14027 = CARTESIAN_POINT ( 'NONE',  ( 11.24999999999999645, 3.073863465859856794E-15, -25.10000000000000142 ) ) ;
#14028 = DIRECTION ( 'NONE',  ( -0.000000000000000000, 1.000000000000000000, -0.000000000000000000 ) ) ;
#14029 = PRESENTATION_STYLE_ASSIGNMENT (( #12407 ) ) ;
#14030 = DIRECTION ( 'NONE',  ( 0.000000000000000000, 0.000000000000000000, 1.000000000000000000 ) ) ;
#14031 = DIRECTION ( 'NONE',  ( -0.000000000000000000, 1.000000000000000000, -0.000000000000000000 ) ) ;
#14032 = CARTESIAN_POINT ( 'NONE',  ( 0.000000000000000000, 29.03656532225563680, 15.68049343256006800 ) ) ;
#14033 = EDGE_LOOP ( 'NONE', ( #14310, #4520, #3955, #13805 ) ) ;
#14034 = DIRECTION ( 'NONE',  ( -1.000000000000000000, -0.000000000000000000, -0.000000000000000000 ) ) ;
#14035 = ORIENTED_EDGE ( 'NONE', *, *, #1308, .F. ) ;
#14036 = EDGE_CURVE ( 'NONE', #12396, #14252, #14778, .T. ) ;
#14037 = CARTESIAN_POINT ( 'NONE',  ( 2.100000000000000089, 0.000000000000000000, -5.000000000000000000 ) ) ;
#14038 = CARTESIAN_POINT ( 'NONE',  ( 34.99999999999999289, 0.000000000000000000, 0.000000000000000000 ) ) ;
#14039 = VERTEX_POINT ( 'NONE', #4144 ) ;
#14040 = ORIENTED_EDGE ( 'NONE', *, *, #2281, .F. ) ;
#14041 = CYLINDRICAL_SURFACE ( 'NONE', #12984, 63.00000000006298961 ) ;
#14042 = AXIS2_PLACEMENT_3D ( 'NONE', #10155, #14534, #1497 ) ;
#14043 = CARTESIAN_POINT ( 'NONE',  ( 10.00000000000000000, 5.940243314904215310, 32.46095361140694990 ) ) ;
#14044 = ORIENTED_EDGE ( 'NONE', *, *, #4492, .T. ) ;
#14045 = ADVANCED_FACE ( 'NONE', ( #1558 ), #10221, .T. ) ;
#14046 = B_SPLINE_CURVE_WITH_KNOTS ( 'NONE', 3,
 ( #961, #13911, #6760, #2189, #7996, #9614 ),
 .UNSPECIFIED., .F., .F.,
 ( 4, 2, 4 ),
 ( 0.003358874760055551890, 0.004541967308452098118, 0.005725059856848645212 ),
 .UNSPECIFIED. ) ;
#14047 = CARTESIAN_POINT ( 'NONE',  ( -26.29305231718584324, -26.50000000000000000, 16.45302069950530566 ) ) ;
#14048 = DIRECTION ( 'NONE',  ( 0.000000000000000000, 0.000000000000000000, 1.000000000000000000 ) ) ;
#14049 = PLANE ( 'NONE',  #847 ) ;
#14050 = DIRECTION ( 'NONE',  ( 0.000000000000000000, 0.000000000000000000, 1.000000000000000000 ) ) ;
#14051 = ORIENTED_EDGE ( 'NONE', *, *, #16713, .T. ) ;
#14052 = CARTESIAN_POINT ( 'NONE',  ( -90.00000000009001155, -13.00000000000001776, -5.000000000000005329 ) ) ;
#14053 = ORIENTED_EDGE ( 'NONE', *, *, #12800, .F. ) ;
#14054 = VECTOR ( 'NONE', #14660, 1000.000000000000000 ) ;
#14055 = CARTESIAN_POINT ( 'NONE',  ( 4.211140560182196957, 2.431303136016536470, -3.745885042887433514 ) ) ;
#14056 = DIRECTION ( 'NONE',  ( -1.000000000000000000, 0.000000000000000000, 0.000000000000000000 ) ) ;
#14057 = CARTESIAN_POINT ( 'NONE',  ( 10.00000000000000000, 44.70888270294211253, -34.13306034420136825 ) ) ;
#14058 = ORIENTED_EDGE ( 'NONE', *, *, #15890, .T. ) ;
#14059 = ORIENTED_EDGE ( 'NONE', *, *, #15191, .T. ) ;
#14060 = CARTESIAN_POINT ( 'NONE',  ( 0.000000000000000000, 13.24999999999999822, 0.000000000000000000 ) ) ;
#14061 =( NAMED_UNIT ( * ) SI_UNIT ( $, .STERADIAN. ) SOLID_ANGLE_UNIT ( ) );
#14062 = VERTEX_POINT ( 'NONE', #7083 ) ;
#14063 = DIRECTION ( 'NONE',  ( -1.000000000000000000, -0.000000000000000000, -0.000000000000000000 ) ) ;
#14064 = EDGE_CURVE ( 'NONE', #3708, #13893, #18423, .T. ) ;
#14065 = AXIS2_PLACEMENT_3D ( 'NONE', #7981, #1980, #16657 ) ;
#14066 = DIRECTION ( 'NONE',  ( -1.000000000000000000, -0.000000000000000000, -0.000000000000000000 ) ) ;
#14067 = DIRECTION ( 'NONE',  ( -1.000000000000000000, -0.000000000000000000, 0.000000000000000000 ) ) ;
#14068 = ORIENTED_EDGE ( 'NONE', *, *, #8383, .T. ) ;
#14069 = FACE_OUTER_BOUND ( 'NONE', #16800, .T. ) ;
#14070 = ORIENTED_EDGE ( 'NONE', *, *, #7382, .F. ) ;
#14071 = CARTESIAN_POINT ( 'NONE',  ( -0.1410422978106123659, 4.700232962125094893, -3.687027686973624707 ) ) ;
#14072 = LINE ( 'NONE', #9787, #2822 ) ;
#14073 = CARTESIAN_POINT ( 'NONE',  ( 0.000000000000000000, 0.000000000000000000, 0.000000000000000000 ) ) ;
#14074 = EDGE_CURVE ( 'NONE', #7406, #13131, #13868, .T. ) ;
#14075 = VERTEX_POINT ( 'NONE', #4244 ) ;
#14076 = DIRECTION ( 'NONE',  ( 1.000000000000000000, 0.000000000000000000, 0.000000000000000000 ) ) ;
#14077 = ORIENTED_EDGE ( 'NONE', *, *, #6461, .T. ) ;
#14078 = CARTESIAN_POINT ( 'NONE',  ( 2.500000000000000000, -2.357898499370432166, 3.035766082959412415E-15 ) ) ;
#14079 = CARTESIAN_POINT ( 'NONE',  ( 10.00000000000000000, 29.75305054077471922, 14.27431201565535090 ) ) ;
#14080 = VERTEX_POINT ( 'NONE', #8795 ) ;
#14081 = ORIENTED_EDGE ( 'NONE', *, *, #2620, .F. ) ;
#14082 = DIRECTION ( 'NONE',  ( -1.000000000000000000, 0.000000000000000000, 0.000000000000000000 ) ) ;
#14083 = EDGE_CURVE ( 'NONE', #18209, #9028, #10218, .T. ) ;
#14084 = ORIENTED_EDGE ( 'NONE', *, *, #714, .F. ) ;
#14085 = LINE ( 'NONE', #8370, #14285 ) ;
#14086 = AXIS2_PLACEMENT_3D ( 'NONE', #15185, #4605, #17838 ) ;
#14087 = CARTESIAN_POINT ( 'NONE',  ( 10.00000000000000000, 38.81885513160045065, -40.70683587897917022 ) ) ;
#14088 = ORIENTED_EDGE ( 'NONE', *, *, #16510, .T. ) ;
#14089 = ORIENTED_EDGE ( 'NONE', *, *, #17718, .T. ) ;
#14090 = CARTESIAN_POINT ( 'NONE',  ( -79.64793068852927149, -30.00000000000000000, 29.21039329588765554 ) ) ;
#14091 = CARTESIAN_POINT ( 'NONE',  ( 10.00000000000000000, 0.000000000000000000, 0.000000000000000000 ) ) ;
#14092 = DIRECTION ( 'NONE',  ( 1.000000000000000000, 0.000000000000000000, 0.000000000000000000 ) ) ;
#14093 = FACE_OUTER_BOUND ( 'NONE', #2307, .T. ) ;
#14094 = DIRECTION ( 'NONE',  ( -1.000000000000000000, -0.000000000000000000, 0.000000000000000000 ) ) ;
#14095 = DIRECTION ( 'NONE',  ( 0.000000000000000000, 0.000000000000000000, 1.000000000000000000 ) ) ;
#14096 = CARTESIAN_POINT ( 'NONE',  ( 4.024499207728847949, -2.323545700935699454, -3.572172305156873673 ) ) ;
#14097 = ORIENTED_EDGE ( 'NONE', *, *, #2954, .T. ) ;
#14098 = CARTESIAN_POINT ( 'NONE',  ( 10.00000000000000000, 6.681932690257323060, -25.38428207620315291 ) ) ;
#14099 = FACE_OUTER_BOUND ( 'NONE', #18295, .T. ) ;
#14100 = CARTESIAN_POINT ( 'NONE',  ( 1.250000000000000000, -6.429618962271402616, 0.000000000000000000 ) ) ;
#14101 = ORIENTED_EDGE ( 'NONE', *, *, #7270, .F. ) ;
#14102 = VECTOR ( 'NONE', #12413, 1000.000000000000114 ) ;
#14103 = VERTEX_POINT ( 'NONE', #1373 ) ;
#14104 = ORIENTED_EDGE ( 'NONE', *, *, #1925, .F. ) ;
#14105 = ADVANCED_FACE ( 'NONE', ( #18614 ), #12999, .T. ) ;
#14106 = ORIENTED_EDGE ( 'NONE', *, *, #14936, .F. ) ;
#14107 = DIRECTION ( 'NONE',  ( 1.000000000000000000, 0.000000000000000000, 0.000000000000000000 ) ) ;
#14108 = EDGE_CURVE ( 'NONE', #10818, #6404, #12043, .T. ) ;
#14109 = LINE ( 'NONE', #2691, #8824 ) ;
#14110 = DIRECTION ( 'NONE',  ( -0.000000000000000000, -1.000000000000000000, -0.000000000000000000 ) ) ;
#14111 = DIRECTION ( 'NONE',  ( 0.000000000000000000, 0.000000000000000000, 1.000000000000000000 ) ) ;
#14112 = CARTESIAN_POINT ( 'NONE',  ( 10.00000000000000000, 0.000000000000000000, 0.000000000000000000 ) ) ;
#14113 = STYLED_ITEM ( 'NONE', ( #3079 ), #5356 ) ;
#14114 = ADVANCED_FACE ( 'NONE', ( #7000, #16036, #14607, #11573, #17103, #5659, #11475 ), #2803, .F. ) ;
#14115 = DIRECTION ( 'NONE',  ( -0.000000000000000000, 1.000000000000000000, -0.000000000000000000 ) ) ;
#14116 = CARTESIAN_POINT ( 'NONE',  ( 0.000000000000000000, 0.000000000000000000, 0.000000000000000000 ) ) ;
#14117 = FACE_OUTER_BOUND ( 'NONE', #2221, .T. ) ;
#14118 = ORIENTED_EDGE ( 'NONE', *, *, #3526, .T. ) ;
#14119 = DIRECTION ( 'NONE',  ( 0.000000000000000000, 0.000000000000000000, 1.000000000000000000 ) ) ;
#14120 = ORIENTED_EDGE ( 'NONE', *, *, #14693, .F. ) ;
#14121 = EDGE_CURVE ( 'NONE', #14354, #12355, #17796, .T. ) ;
#14122 = CARTESIAN_POINT ( 'NONE',  ( 10.00000000000000000, 13.79392154159223693, -61.47135697633763129 ) ) ;
#14123 = DIRECTION ( 'NONE',  ( -1.000000000000000000, -0.000000000000000000, -0.000000000000000000 ) ) ;
#14124 = ORIENTED_EDGE ( 'NONE', *, *, #10569, .F. ) ;
#14125 = DIRECTION ( 'NONE',  ( 0.000000000000000000, 0.000000000000000000, 1.000000000000000000 ) ) ;
#14126 = APPLICATION_PROTOCOL_DEFINITION ( 'draft international standard', 'automotive_design', 1998, #9864 ) ;
#14127 = DIRECTION ( 'NONE',  ( -0.000000000000000000, -0.000000000000000000, -1.000000000000000000 ) ) ;
#14128 = EDGE_LOOP ( 'NONE', ( #13209, #15610 ) ) ;
#14129 = EDGE_CURVE ( 'NONE', #1653, #18126, #8398, .T. ) ;
#14130 = STYLED_ITEM ( 'NONE', ( #14643 ), #8303 ) ;
#14131 = AXIS2_PLACEMENT_3D ( 'NONE', #5211, #18069, #6651 ) ;
#14132 = EDGE_CURVE ( 'NONE', #15913, #9305, #12659, .T. ) ;
#14133 = CARTESIAN_POINT ( 'NONE',  ( 0.000000000000000000, -29.03656532225574338, 15.68049343255986372 ) ) ;
#14134 = EDGE_CURVE ( 'NONE', #10364, #17129, #17463, .T. ) ;
#14135 = DIRECTION ( 'NONE',  ( 0.000000000000000000, 0.000000000000000000, 1.000000000000000000 ) ) ;
#14136 = DIRECTION ( 'NONE',  ( -1.000000000000000000, 0.000000000000000000, -0.000000000000000000 ) ) ;
#14137 = DIRECTION ( 'NONE',  ( 1.000000000000000000, 0.000000000000000000, 0.000000000000000000 ) ) ;
#14138 = EDGE_CURVE ( 'NONE', #2861, #11226, #15662, .T. ) ;
#14139 = UNCERTAINTY_MEASURE_WITH_UNIT (LENGTH_MEASURE( 1.000000000000000082E-05 ), #8004, 'distance_accuracy_value', 'NONE');
#14140 = CARTESIAN_POINT ( 'NONE',  ( 2.500000000000000000, 0.000000000000000000, 0.000000000000000000 ) ) ;
#14141 = ORIENTED_EDGE ( 'NONE', *, *, #14129, .T. ) ;
#14142 = EDGE_CURVE ( 'NONE', #15913, #18678, #4150, .T. ) ;
#14143 = COLOUR_RGB ( '',1.000000000000000000, 0.9490196078431372140, 0.9098039215686274384 ) ;
#14144 = CYLINDRICAL_SURFACE ( 'NONE', #2317, 24.00000000002399503 ) ;
#14145 = DIRECTION ( 'NONE',  ( -1.000000000000000000, -0.000000000000000000, -0.000000000000000000 ) ) ;
#14146 = CARTESIAN_POINT ( 'NONE',  ( 4.999999999999999112, 61.47135697633778051, 13.79392154159156370 ) ) ;
#14147 = EDGE_LOOP ( 'NONE', ( #15283, #8591, #16361, #16461 ) ) ;
#14148 = AXIS2_PLACEMENT_3D ( 'NONE', #14531, #13201, #4433 ) ;
#14149 = ORIENTED_EDGE ( 'NONE', *, *, #3310, .T. ) ;
#14150 = TOROIDAL_SURFACE ( 'NONE', #16579, 25.10000000000000142, 0.09999999999999766020 ) ;
#14151 = DIRECTION ( 'NONE',  ( 0.000000000000000000, 0.000000000000000000, 1.000000000000000000 ) ) ;
#14152 = SURFACE_STYLE_USAGE ( .BOTH. , #6915 ) ;
#14153 = ORIENTED_EDGE ( 'NONE', *, *, #6114, .T. ) ;
#14154 = DIRECTION ( 'NONE',  ( -1.000000000000000000, -0.000000000000000000, 0.000000000000000000 ) ) ;
#14155 = AXIS2_PLACEMENT_3D ( 'NONE', #8419, #6613, #13840 ) ;
#14156 = DIRECTION ( 'NONE',  ( 1.000000000000000000, 0.000000000000000000, -0.000000000000000000 ) ) ;
#14157 = AXIS2_PLACEMENT_3D ( 'NONE', #13019, #16060, #9280 ) ;
#14159 = CIRCLE ( 'NONE', #1107, 24.00000000002399858 ) ;
#14158 = DIRECTION ( 'NONE',  ( 0.000000000000000000, 0.000000000000000000, -1.000000000000000000 ) ) ;
#14160 = VERTEX_POINT ( 'NONE', #13267 ) ;
#14161 = CYLINDRICAL_SURFACE ( 'NONE', #663, 24.00000000002399503 ) ;
#14162 = ORIENTED_EDGE ( 'NONE', *, *, #524, .T. ) ;
#14164 = CARTESIAN_POINT ( 'NONE',  ( 0.2499999999999966416, -8.096141056083448362, -1.000000000000000000 ) ) ;
#14163 = UNCERTAINTY_MEASURE_WITH_UNIT (LENGTH_MEASURE( 1.000000000000000082E-05 ), #3316, 'distance_accuracy_value', 'NONE');
#14165 = CYLINDRICAL_SURFACE ( 'NONE', #13825, 4.349594641156947716 ) ;
#14166 = DIRECTION ( 'NONE',  ( -0.000000000000000000, 1.000000000000000000, 1.224646799147353207E-16 ) ) ;
#14167 = ORIENTED_EDGE ( 'NONE', *, *, #5395, .F. ) ;
#14168 = DIRECTION ( 'NONE',  ( 0.000000000000000000, 0.000000000000000000, 1.000000000000000000 ) ) ;
#14169 = EDGE_CURVE ( 'NONE', #5321, #6853, #17519, .T. ) ;
#14170 = EDGE_LOOP ( 'NONE', ( #18572, #15020, #8924, #14752 ) ) ;
#14171 = CARTESIAN_POINT ( 'NONE',  ( -90.40196296004810961, 1.745901168134654787E-14, 6.951864913735149365 ) ) ;
#14172 = LINE ( 'NONE', #11021, #7077 ) ;
#14173 = AXIS2_PLACEMENT_3D ( 'NONE', #8531, #17475, #13110 ) ;
#14174 = ORIENTED_EDGE ( 'NONE', *, *, #13315, .T. ) ;
#14175 = ORIENTED_EDGE ( 'NONE', *, *, #17564, .F. ) ;
#14176 = CYLINDRICAL_SURFACE ( 'NONE', #9319, 26.24900000002624978 ) ;
#14177 = AXIS2_PLACEMENT_3D ( 'NONE', #4872, #3450, #3258 ) ;
#14178 = EDGE_LOOP ( 'NONE', ( #11967, #13012, #2605, #6713 ) ) ;
#14179 = FACE_OUTER_BOUND ( 'NONE', #15495, .T. ) ;
#14180 = DIRECTION ( 'NONE',  ( 0.000000000000000000, 0.000000000000000000, 1.000000000000000000 ) ) ;
#14181 = AXIS2_PLACEMENT_3D ( 'NONE', #12116, #3457, #11746 ) ;
#14182 = AXIS2_PLACEMENT_3D ( 'NONE', #6856, #2568, #10006 ) ;
#14183 = ADVANCED_FACE ( 'NONE', ( #13372 ), #1640, .F. ) ;
#14184 = AXIS2_PLACEMENT_3D ( 'NONE', #15563, #1190, #6891 ) ;
#14185 = VECTOR ( 'NONE', #9314, 1000.000000000000000 ) ;
#14186 = EDGE_LOOP ( 'NONE', ( #3629, #14051, #6528, #6491 ) ) ;
#14187 = EDGE_CURVE ( 'NONE', #8908, #9439, #1836, .T. ) ;
#14188 = AXIS2_PLACEMENT_3D ( 'NONE', #14217, #6874, #12693 ) ;
#14189 = VECTOR ( 'NONE', #10870, 1000.000000000000000 ) ;
#14190 = EDGE_LOOP ( 'NONE', ( #15258, #14926, #14341, #1934, #2972 ) ) ;
#14191 = DIRECTION ( 'NONE',  ( -0.000000000000000000, 1.000000000000000000, -0.000000000000000000 ) ) ;
#14192 = AXIS2_PLACEMENT_3D ( 'NONE', #6061, #6152, #165 ) ;
#14193 = DIRECTION ( 'NONE',  ( -1.000000000000000000, -0.000000000000000000, -0.000000000000000000 ) ) ;
#14194 = FACE_OUTER_BOUND ( 'NONE', #12703, .T. ) ;
#14195 = DIRECTION ( 'NONE',  ( -1.000000000000000000, 0.000000000000000000, -0.000000000000000000 ) ) ;
#14196 = CARTESIAN_POINT ( 'NONE',  ( 5.000000000000000000, 22.76987570971527575, 23.88582760061489552 ) ) ;
#14197 = DIRECTION ( 'NONE',  ( -1.000000000000000000, 0.000000000000000000, 0.000000000000000000 ) ) ;
#14198 = DIRECTION ( 'NONE',  ( 0.000000000000000000, 0.000000000000000000, 1.000000000000000000 ) ) ;
#14199 = EDGE_LOOP ( 'NONE', ( #9866, #11628 ) ) ;
#14200 = DIRECTION ( 'NONE',  ( -1.000000000000000000, -0.000000000000000000, -0.000000000000000000 ) ) ;
#14201 = CARTESIAN_POINT ( 'NONE',  ( 10.00000000000000000, 0.000000000000000000, 0.000000000000000000 ) ) ;
#14202 = CARTESIAN_POINT ( 'NONE',  ( 23.50000000000000355, 0.000000000000000000, 0.000000000000000000 ) ) ;
#14203 = FACE_OUTER_BOUND ( 'NONE', #7346, .T. ) ;
#14204 = CIRCLE ( 'NONE', #5974, 2.500000000000000888 ) ;
#14205 = AXIS2_PLACEMENT_3D ( 'NONE', #15803, #2754, #4280 ) ;
#14206 = AXIS2_PLACEMENT_3D ( 'NONE', #12194, #772, #5142 ) ;
#14207 = ORIENTED_EDGE ( 'NONE', *, *, #966, .F. ) ;
#14208 = VECTOR ( 'NONE', #16063, 1000.000000000000000 ) ;
#14209 = AXIS2_PLACEMENT_3D ( 'NONE', #9848, #17008, #11368 ) ;
#14210 = EDGE_CURVE ( 'NONE', #6839, #10560, #6569, .T. ) ;
#14211 = VERTEX_POINT ( 'NONE', #11840 ) ;
#14212 = CYLINDRICAL_SURFACE ( 'NONE', #13001, 26.24900000002624978 ) ;
#14213 = FACE_OUTER_BOUND ( 'NONE', #18281, .T. ) ;
#14214 = CIRCLE ( 'NONE', #7810, 63.00000000006298961 ) ;
#14215 = EDGE_LOOP ( 'NONE', ( #6036, #11009, #11314, #3438 ) ) ;
#14216 = DIRECTION ( 'NONE',  ( 0.000000000000000000, 0.000000000000000000, -1.000000000000000000 ) ) ;
#14217 = CARTESIAN_POINT ( 'NONE',  ( 10.00000000000000000, 24.68609584167230153, -50.69000562871616467 ) ) ;
#14218 = AXIS2_PLACEMENT_3D ( 'NONE', #6172, #13708, #14944 ) ;
#14219 = DIRECTION ( 'NONE',  ( -1.000000000000000000, 0.000000000000000000, 0.000000000000000000 ) ) ;
#14220 = DIRECTION ( 'NONE',  ( -1.000000000000000000, -0.000000000000000000, -0.000000000000000000 ) ) ;
#14221 = AXIS2_PLACEMENT_3D ( 'NONE', #17863, #10706, #8995 ) ;
#14222 = DIRECTION ( 'NONE',  ( -1.000000000000000000, -0.000000000000000000, -0.000000000000000000 ) ) ;
#14223 = ORIENTED_EDGE ( 'NONE', *, *, #14083, .T. ) ;
#14224 = VECTOR ( 'NONE', #3091, 1000.000000000000000 ) ;
#14225 = CARTESIAN_POINT ( 'NONE',  ( 5.000000000000000000, 32.70783759231086663, 4.381479206523104963 ) ) ;
#14226 = EDGE_LOOP ( 'NONE', ( #9772, #12378, #11891, #10690 ) ) ;
#14227 = DIRECTION ( 'NONE',  ( 0.000000000000000000, 0.000000000000000000, 1.000000000000000000 ) ) ;
#14228 = DIRECTION ( 'NONE',  ( 0.000000000000000000, -1.000000000000000000, 0.000000000000000000 ) ) ;
#14229 = VERTEX_POINT ( 'NONE', #14692 ) ;
#14230 = ADVANCED_FACE ( 'NONE', ( #3086 ), #3366, .T. ) ;
#14231 = DIRECTION ( 'NONE',  ( -1.000000000000000000, -0.000000000000000000, -0.000000000000000000 ) ) ;
#14232 = DIRECTION ( 'NONE',  ( 2.805047682034665168E-18, -1.000000000000000000, 1.351931264281300807E-16 ) ) ;
#14234 = ADVANCED_FACE ( 'NONE', ( #3269 ), #5034, .F. ) ;
#14233 = DIRECTION ( 'NONE',  ( -1.000000000000000000, 0.000000000000000000, -0.000000000000000000 ) ) ;
#14235 = ORIENTED_EDGE ( 'NONE', *, *, #15764, .T. ) ;
#14236 = AXIS2_PLACEMENT_3D ( 'NONE', #4078, #8545, #1586 ) ;
#14237 = CIRCLE ( 'NONE', #14524, 33.00000000003299760 ) ;
#14238 = AXIS2_PLACEMENT_3D ( 'NONE', #9253, #11843, #15076 ) ;
#14239 = VECTOR ( 'NONE', #604, 1000.000000000000000 ) ;
#14240 = DIRECTION ( 'NONE',  ( 1.000000000000000000, 0.000000000000000000, 0.000000000000000000 ) ) ;
#14241 = CARTESIAN_POINT ( 'NONE',  ( 0.9999999999999997780, -27.60846790388774608, -2.000000000000000000 ) ) ;
#14242 = DIRECTION ( 'NONE',  ( -1.000000000000000000, -0.000000000000000000, -0.000000000000000000 ) ) ;
#14243 = DIRECTION ( 'NONE',  ( 0.000000000000000000, 0.9510565162951544194, -0.3090169943749447312 ) ) ;
#14244 = EDGE_CURVE ( 'NONE', #18322, #18738, #13265, .T. ) ;
#14245 = CARTESIAN_POINT ( 'NONE',  ( 10.00000000000000000, 6.681932690256967788, 25.38428207620324883 ) ) ;
#14246 = ORIENTED_EDGE ( 'NONE', *, *, #4832, .T. ) ;
#14247 = VECTOR ( 'NONE', #4592, 1000.000000000000000 ) ;
#14248 = DIRECTION ( 'NONE',  ( -1.000000000000000000, 0.000000000000000000, 0.000000000000000000 ) ) ;
#14249 = DIRECTION ( 'NONE',  ( 0.000000000000000000, 0.000000000000000000, 1.000000000000000000 ) ) ;
#14250 = DIRECTION ( 'NONE',  ( 0.000000000000000000, -0.3090169943749546677, 0.9510565162951511997 ) ) ;
#14251 = VECTOR ( 'NONE', #9352, 1000.000000000000000 ) ;
#14252 = VERTEX_POINT ( 'NONE', #132 ) ;
#14253 = EDGE_LOOP ( 'NONE', ( #13228, #8346, #897, #15199 ) ) ;
#14254 = VECTOR ( 'NONE', #881, 1000.000000000000000 ) ;
#14255 = EDGE_CURVE ( 'NONE', #13366, #7648, #11929, .T. ) ;
#14256 = CARTESIAN_POINT ( 'NONE',  ( -117.1020693116508085, -34.99999999999999289, 19.69080595179778115 ) ) ;
#14257 = ADVANCED_FACE ( 'NONE', ( #1738 ), #17558, .T. ) ;
#14258 = ADVANCED_FACE ( 'NONE', ( #4686 ), #16135, .T. ) ;
#14259 = ORIENTED_EDGE ( 'NONE', *, *, #1244, .T. ) ;
#14260 = FACE_OUTER_BOUND ( 'NONE', #14215, .T. ) ;
#14261 = ADVANCED_FACE ( 'NONE', ( #9072 ), #8879, .T. ) ;
#14262 = AXIS2_PLACEMENT_3D ( 'NONE', #4607, #17747, #10415 ) ;
#14263 = EDGE_CURVE ( 'NONE', #12365, #4436, #9631, .T. ) ;
#14264 = CIRCLE ( 'NONE', #12433, 24.00000000002399858 ) ;
#14265 = PLANE ( 'NONE',  #8676 ) ;
#14266 = AXIS2_PLACEMENT_3D ( 'NONE', #2363, #5308, #3991 ) ;
#14267 = CARTESIAN_POINT ( 'NONE',  ( 0.000000000000000000, 0.000000000000000000, -5.000000000000000000 ) ) ;
#14268 =( REPRESENTATION_RELATIONSHIP ('NONE','NONE', #11014, #8256 ) REPRESENTATION_RELATIONSHIP_WITH_TRANSFORMATION ( #9247 )SHAPE_REPRESENTATION_RELATIONSHIP( ) );
#14269 = EDGE_LOOP ( 'NONE', ( #16433, #11304, #15703, #15697 ) ) ;
#14270 =( NAMED_UNIT ( * ) PLANE_ANGLE_UNIT ( ) SI_UNIT ( $, .RADIAN. ) );
#14271 = ADVANCED_FACE ( 'NONE', ( #4882 ), #499, .T. ) ;
#14272 = ORIENTED_EDGE ( 'NONE', *, *, #6779, .F. ) ;
#14273 = CARTESIAN_POINT ( 'NONE',  ( 4.888507282057958925, -29.45674523562211888, 0.000000000000000000 ) ) ;
#14274 = DIRECTION ( 'NONE',  ( 0.000000000000000000, 0.000000000000000000, 1.000000000000000000 ) ) ;
#14275 = CYLINDRICAL_SURFACE ( 'NONE', #17880, 24.00000000002399858 ) ;
#14276 = ORIENTED_EDGE ( 'NONE', *, *, #4418, .F. ) ;
#14277 = DIRECTION ( 'NONE',  ( -0.000000000000000000, 0.000000000000000000, 1.000000000000000000 ) ) ;
#14278 = ORIENTED_EDGE ( 'NONE', *, *, #11237, .F. ) ;
#14279 = CYLINDRICAL_SURFACE ( 'NONE', #5458, 24.00000000002400213 ) ;
#14280 = FACE_OUTER_BOUND ( 'NONE', #10892, .T. ) ;
#14281 = ORIENTED_EDGE ( 'NONE', *, *, #17971, .T. ) ;
#14282 = VERTEX_POINT ( 'NONE', #10681 ) ;
#14283 = EDGE_CURVE ( 'NONE', #17827, #5885, #17839, .T. ) ;
#14284 = CARTESIAN_POINT ( 'NONE',  ( 0.000000000000000000, -1.017308535512791767, 56.37237871411032586 ) ) ;
#14285 = VECTOR ( 'NONE', #8282, 1000.000000000000000 ) ;
#14286 = VERTEX_POINT ( 'NONE', #16414 ) ;
#14287 = CARTESIAN_POINT ( 'NONE',  ( 5.000000000000004441, 0.000000000000000000, 0.000000000000000000 ) ) ;
#14288 = DIRECTION ( 'NONE',  ( 0.000000000000000000, 0.000000000000000000, -1.000000000000000000 ) ) ;
#14289 = EDGE_CURVE ( 'NONE', #18064, #15756, #10963, .T. ) ;
#14290 = AXIS2_PLACEMENT_3D ( 'NONE', #13919, #4956, #9333 ) ;
#14291 = VERTEX_POINT ( 'NONE', #15549 ) ;
#14292 = VECTOR ( 'NONE', #7768, 1000.000000000000000 ) ;
#14293 = VERTEX_POINT ( 'NONE', #12587 ) ;
#14294 = DIRECTION ( 'NONE',  ( 0.000000000000000000, 0.1564344650402312298, -0.9876883405951376593 ) ) ;
#14295 = DIRECTION ( 'NONE',  ( -1.000000000000000000, -0.000000000000000000, 0.000000000000000000 ) ) ;
#14296 = DIRECTION ( 'NONE',  ( 0.000000000000000000, 0.000000000000000000, 1.000000000000000000 ) ) ;
#14297 = LINE ( 'NONE', #4010, #5066 ) ;
#14298 = CARTESIAN_POINT ( 'NONE',  ( 11.14999999999999680, 0.000000000000000000, 0.000000000000000000 ) ) ;
#14299 = DIRECTION ( 'NONE',  ( 0.000000000000000000, -0.7071067811865389130, -0.7071067811865561215 ) ) ;
#14300 = DIRECTION ( 'NONE',  ( 0.000000000000000000, 0.9510565162951543083, -0.3090169943749447867 ) ) ;
#14301 = ORIENTED_EDGE ( 'NONE', *, *, #5157, .F. ) ;
#14302 = LINE ( 'NONE', #14098, #4544 ) ;
#14303 = LINE ( 'NONE', #12579, #7173 ) ;
#14304 = DIRECTION ( 'NONE',  ( 0.000000000000000000, 1.000000000000000000, -1.287488025362403787E-15 ) ) ;
#14305 = AXIS2_PLACEMENT_3D ( 'NONE', #8527, #8619, #13236 ) ;
#14306 = DIRECTION ( 'NONE',  ( -1.000000000000000000, -0.000000000000000000, 0.000000000000000000 ) ) ;
#14307 = AXIS2_PLACEMENT_3D ( 'NONE', #1006, #17192, #1374 ) ;
#14308 = EDGE_LOOP ( 'NONE', ( #13025, #9829, #7205, #13728 ) ) ;
#14309 = ADVANCED_FACE ( 'NONE', ( #16985 ), #6781, .T. ) ;
#14310 = ORIENTED_EDGE ( 'NONE', *, *, #2726, .T. ) ;
#14311 = DIRECTION ( 'NONE',  ( 0.000000000000000000, -0.4999999999999993339, 0.8660254037844390407 ) ) ;
#14312 = FILL_AREA_STYLE ('',( #1176 ) ) ;
#14313 = ORIENTED_EDGE ( 'NONE', *, *, #17503, .F. ) ;
#14314 = AXIS2_PLACEMENT_3D ( 'NONE', #229, #4413, #411 ) ;
#14315 = LINE ( 'NONE', #4035, #3010 ) ;
#14316 = DIRECTION ( 'NONE',  ( 1.000000000000000000, -2.312964634635740492E-16, 0.000000000000000000 ) ) ;
#14317 = CARTESIAN_POINT ( 'NONE',  ( 10.00000000000000000, -34.13306034420153168, -44.70888270294199884 ) ) ;
#14318 = CARTESIAN_POINT ( 'NONE',  ( -117.1020693116508085, -30.00000000000000000, 19.69080595179778115 ) ) ;
#14319 = DIRECTION ( 'NONE',  ( 0.000000000000000000, -0.5000000000000009992, -0.8660254037844380415 ) ) ;
#14320 = ORIENTED_EDGE ( 'NONE', *, *, #704, .T. ) ;
#14321 = CARTESIAN_POINT ( 'NONE',  ( -4.000000000000000000, 0.9868501483902560878, -0.09357334158579519445 ) ) ;
#14322 = EDGE_LOOP ( 'NONE', ( #11924, #2168, #8278, #1135 ) ) ;
#14323 = EDGE_CURVE ( 'NONE', #872, #18209, #1418, .T. ) ;
#14324 = DIRECTION ( 'NONE',  ( 0.000000000000000000, 0.000000000000000000, 1.000000000000000000 ) ) ;
#14325 = DIRECTION ( 'NONE',  ( -1.000000000000000000, -0.000000000000000000, 0.000000000000000000 ) ) ;
#14326 = EDGE_LOOP ( 'NONE', ( #17213, #16045, #11131, #12900 ) ) ;
#14327 = EDGE_CURVE ( 'NONE', #17735, #8855, #18301, .T. ) ;
#14328 = CARTESIAN_POINT ( 'NONE',  ( 11.14999999999999680, 3.673940397442059967E-15, -30.00000000000000711 ) ) ;
#14329 = EDGE_LOOP ( 'NONE', ( #12256, #9169, #13029, #12153 ) ) ;
#14330 = CARTESIAN_POINT ( 'NONE',  ( 0.000000000000000000, 56.37237871411034007, 1.017308535512583711 ) ) ;
#14331 = CARTESIAN_POINT ( 'NONE',  ( 2.500000000000000000, 2.357898499370432166, -2.385244779468109755E-15 ) ) ;
#14332 = DIRECTION ( 'NONE',  ( 1.000000000000000000, 0.000000000000000000, 0.000000000000000000 ) ) ;
#14333 = DIRECTION ( 'NONE',  ( 0.000000000000000000, -1.000000000000000000, 1.287488025362403787E-15 ) ) ;
#14334 = CARTESIAN_POINT ( 'NONE',  ( -3.500000000000000888, -27.60846790388774608, -2.000000000000000000 ) ) ;
#14335 = ORIENTED_EDGE ( 'NONE', *, *, #7147, .T. ) ;
#14336 = CIRCLE ( 'NONE', #16774, 12.00000000001200462 ) ;
#14337 = CYLINDRICAL_SURFACE ( 'NONE', #16601, 24.00000000002400213 ) ;
#14338 = LINE ( 'NONE', #7092, #15317 ) ;
#14339 = CARTESIAN_POINT ( 'NONE',  ( 0.000000000000000000, 23.24033432160521429, -58.55669782892436359 ) ) ;
#14340 = ORIENTED_EDGE ( 'NONE', *, *, #4649, .F. ) ;
#14341 = ORIENTED_EDGE ( 'NONE', *, *, #13205, .T. ) ;
#14342 = DIRECTION ( 'NONE',  ( 0.000000000000000000, 0.000000000000000000, 1.000000000000000000 ) ) ;
#14343 = EDGE_LOOP ( 'NONE', ( #777, #10867, #16782, #2664 ) ) ;
#14344 = CARTESIAN_POINT ( 'NONE',  ( 2.500000000000000000, -1.178949249685214307, 2.042000000000001592 ) ) ;
#14345 = FACE_BOUND ( 'NONE', #10573, .T. ) ;
#14346 = DIRECTION ( 'NONE',  ( -0.000000000000000000, 1.000000000000000000, -0.000000000000000000 ) ) ;
#14347 = EDGE_CURVE ( 'NONE', #10957, #13630, #9535, .T. ) ;
#14348 = VERTEX_POINT ( 'NONE', #6694 ) ;
#14349 = ADVANCED_FACE ( 'NONE', ( #8116 ), #5060, .T. ) ;
#14350 = CARTESIAN_POINT ( 'NONE',  ( 0.000000000000000000, -7.478235706488566059, -55.74967257055892134 ) ) ;
#14351 = AXIS2_PLACEMENT_3D ( 'NONE', #12504, #3657, #2213 ) ;
#14352 = EDGE_CURVE ( 'NONE', #8908, #11347, #819, .T. ) ;
#14353 = CIRCLE ( 'NONE', #7056, 24.00000000002399858 ) ;
#14354 = VERTEX_POINT ( 'NONE', #597 ) ;
#14355 = CARTESIAN_POINT ( 'NONE',  ( 0.000000000000000000, -24.79895094899269026, 13.40641754777657013 ) ) ;
#14356 = ORIENTED_EDGE ( 'NONE', *, *, #3767, .F. ) ;
#14357 = DIRECTION ( 'NONE',  ( -1.000000000000000000, -0.000000000000000000, 0.000000000000000000 ) ) ;
#14358 = VERTEX_POINT ( 'NONE', #11052 ) ;
#14359 = EDGE_CURVE ( 'NONE', #18225, #18700, #1711, .T. ) ;
#14360 = DIRECTION ( 'NONE',  ( -0.000000000000000000, 1.000000000000000000, -0.000000000000000000 ) ) ;
#14361 = CARTESIAN_POINT ( 'NONE',  ( 10.00000000000000000, 0.000000000000000000, 0.000000000000000000 ) ) ;
#14362 = VERTEX_POINT ( 'NONE', #982 ) ;
#14363 = ORIENTED_EDGE ( 'NONE', *, *, #16775, .T. ) ;
#14364 = DIRECTION ( 'NONE',  ( -1.000000000000000000, -0.000000000000000000, -0.000000000000000000 ) ) ;
#14365 = EDGE_CURVE ( 'NONE', #931, #6749, #5159, .T. ) ;
#14366 = AXIS2_PLACEMENT_3D ( 'NONE', #13483, #10615, #17757 ) ;
#14367 = ORIENTED_EDGE ( 'NONE', *, *, #14327, .F. ) ;
#14368 = CARTESIAN_POINT ( 'NONE',  ( 0.000000000000000000, 0.000000000000000000, -4.000000000000000000 ) ) ;
#14369 = AXIS2_PLACEMENT_3D ( 'NONE', #2673, #16966, #6855 ) ;
#14370 = EDGE_CURVE ( 'NONE', #11328, #16693, #14501, .T. ) ;
#14371 = APPLICATION_CONTEXT ( 'automotive_design' ) ;
#14372 = CARTESIAN_POINT ( 'NONE',  ( -117.1020693116506379, -30.00000000000000000, -19.69080595179801207 ) ) ;
#14373 = ORIENTED_EDGE ( 'NONE', *, *, #11350, .T. ) ;
#14374 = EDGE_CURVE ( 'NONE', #17109, #2107, #5365, .T. ) ;
#14375 = ORIENTED_EDGE ( 'NONE', *, *, #8068, .F. ) ;
#14376 = CARTESIAN_POINT ( 'NONE',  ( 0.000000000000000000, 0.5192545390863916310, -1.000000000000000000 ) ) ;
#14377 = CARTESIAN_POINT ( 'NONE',  ( -11.15000000000000391, 0.000000000000000000, 0.000000000000000000 ) ) ;
#14378 = FACE_OUTER_BOUND ( 'NONE', #14429, .T. ) ;
#14379 = DIRECTION ( 'NONE',  ( -1.000000000000000000, -0.000000000000000000, -0.000000000000000000 ) ) ;
#14380 = AXIS2_PLACEMENT_3D ( 'NONE', #11224, #18362, #17224 ) ;
#14381 = DIRECTION ( 'NONE',  ( 0.000000000000000000, -0.5877852522924802425, 0.8090169943749422332 ) ) ;
#14383 = CIRCLE ( 'NONE', #6470, 12.00000000001200817 ) ;
#14382 = FACE_OUTER_BOUND ( 'NONE', #4451, .T. ) ;
#14384 = DIRECTION ( 'NONE',  ( 0.000000000000000000, 0.000000000000000000, 1.000000000000000000 ) ) ;
#14385 = ORIENTED_EDGE ( 'NONE', *, *, #3017, .F. ) ;
#14386 = AXIS2_PLACEMENT_3D ( 'NONE', #13922, #1063, #3821 ) ;
#14387 = CARTESIAN_POINT ( 'NONE',  ( -2.742827927723112236, -3.035229711105190464, -3.433252694550595230 ) ) ;
#14388 = EDGE_CURVE ( 'NONE', #17682, #4981, #15455, .T. ) ;
#14389 = EDGE_CURVE ( 'NONE', #13928, #18209, #9348, .T. ) ;
#14390 = ORIENTED_EDGE ( 'NONE', *, *, #8347, .T. ) ;
#14391 = CARTESIAN_POINT ( 'NONE',  ( 0.000000000000000000, 1.178949249685213863, -2.042000000000001148 ) ) ;
#14392 = CARTESIAN_POINT ( 'NONE',  ( 50.00005079999999680, 0.000000000000000000, 0.000000000000000000 ) ) ;
#14393 = VERTEX_POINT ( 'NONE', #15176 ) ;
#14394 = CIRCLE ( 'NONE', #7992, 27.00000000000000000 ) ;
#14395 = VECTOR ( 'NONE', #17799, 1000.000000000000000 ) ;
#14396 = ORIENTED_EDGE ( 'NONE', *, *, #17614, .F. ) ;
#14397 = LINE ( 'NONE', #5735, #6587 ) ;
#14398 = DIRECTION ( 'NONE',  ( -1.000000000000000000, 0.000000000000000000, 0.000000000000000000 ) ) ;
#14399 = VERTEX_POINT ( 'NONE', #8220 ) ;
#14400 = DIRECTION ( 'NONE',  ( 0.000000000000000000, 0.000000000000000000, 1.000000000000000000 ) ) ;
#14401 = CARTESIAN_POINT ( 'NONE',  ( 10.00000000000000000, 46.20417134726178432, -32.31183295104722220 ) ) ;
#14402 = LINE ( 'NONE', #11640, #10568 ) ;
#14403 = CARTESIAN_POINT ( 'NONE',  ( 5.200000000000002842, 0.000000000000000000, 0.000000000000000000 ) ) ;
#14404 = DIRECTION ( 'NONE',  ( 1.000000000000000000, 0.000000000000000000, 0.000000000000000000 ) ) ;
#14405 = ORIENTED_EDGE ( 'NONE', *, *, #18656, .T. ) ;
#14406 = DIRECTION ( 'NONE',  ( -0.000000000000000000, 1.000000000000000000, -0.000000000000000000 ) ) ;
#14407 = ORIENTED_EDGE ( 'NONE', *, *, #12451, .T. ) ;
#14408 = EDGE_CURVE ( 'NONE', #13712, #10104, #8716, .T. ) ;
#14409 = AXIS2_PLACEMENT_3D ( 'NONE', #332, #419, #15192 ) ;
#14410 = FACE_OUTER_BOUND ( 'NONE', #15493, .T. ) ;
#14411 = ORIENTED_EDGE ( 'NONE', *, *, #16999, .T. ) ;
#14412 = SHAPE_DEFINITION_REPRESENTATION ( #13485, #16132 ) ;
#14413 = ORIENTED_EDGE ( 'NONE', *, *, #2712, .F. ) ;
#14414 = AXIS2_PLACEMENT_3D ( 'NONE', #6707, #997, #12510 ) ;
#14415 = EDGE_CURVE ( 'NONE', #11596, #1683, #2946, .T. ) ;
#14416 = DIRECTION ( 'NONE',  ( 2.031314180040284764E-16, 1.000000000000000000, 1.301042606982601377E-16 ) ) ;
#14417 = CARTESIAN_POINT ( 'NONE',  ( 0.000000000000000000, 15.00000000000000000, 25.00000000000000000 ) ) ;
#14418 = CYLINDRICAL_SURFACE ( 'NONE', #7535, 56.24900000005625600 ) ;
#14419 = FACE_OUTER_BOUND ( 'NONE', #406, .T. ) ;
#14420 = EDGE_CURVE ( 'NONE', #11226, #17956, #13822, .T. ) ;
#14421 = DIRECTION ( 'NONE',  ( 0.000000000000000000, 0.000000000000000000, 1.000000000000000000 ) ) ;
#14422 = ORIENTED_EDGE ( 'NONE', *, *, #16405, .F. ) ;
#14423 = CARTESIAN_POINT ( 'NONE',  ( 10.00000000000000000, 0.000000000000000000, 0.000000000000000000 ) ) ;
#14424 = CYLINDRICAL_SURFACE ( 'NONE', #8324, 33.00000000003299760 ) ;
#14425 = DIRECTION ( 'NONE',  ( 0.000000000000000000, 0.4539904997395479147, -0.8910065241883673437 ) ) ;
#14426 = EDGE_LOOP ( 'NONE', ( #17101, #7440, #6413, #317 ) ) ;
#14427 = ORIENTED_EDGE ( 'NONE', *, *, #9802, .T. ) ;
#14428 = LINE ( 'NONE', #10196, #18117 ) ;
#14429 = EDGE_LOOP ( 'NONE', ( #16050, #14493, #2755, #2925 ) ) ;
#14430 = FACE_OUTER_BOUND ( 'NONE', #5689, .T. ) ;
#14431 = CARTESIAN_POINT ( 'NONE',  ( 5.200000000000002842, 0.000000000000000000, 2.500000000000000444 ) ) ;
#14432 = ORIENTED_EDGE ( 'NONE', *, *, #16410, .F. ) ;
#14433 = CARTESIAN_POINT ( 'NONE',  ( 0.000000000000000000, -26.20671763660629594, 1.489278925039428936 ) ) ;
#14434 = CIRCLE ( 'NONE', #16928, 2.500000000000000888 ) ;
#14435 = ORIENTED_EDGE ( 'NONE', *, *, #3101, .T. ) ;
#14436 = CARTESIAN_POINT ( 'NONE',  ( 23.48826165280197031, 11.24999999999999467, 0.7426739052322662848 ) ) ;
#14437 = CIRCLE ( 'NONE', #8053, 2.649999999999995914 ) ;
#14438 = ORIENTED_EDGE ( 'NONE', *, *, #14389, .T. ) ;
#14439 = CARTESIAN_POINT ( 'NONE',  ( 10.00000000000000000, 48.50907078259439942, -40.19788616105556400 ) ) ;
#14440 = VERTEX_POINT ( 'NONE', #3649 ) ;
#14441 = DIRECTION ( 'NONE',  ( 0.000000000000000000, 0.000000000000000000, 1.000000000000000000 ) ) ;
#14442 = DIRECTION ( 'NONE',  ( 0.03086419753086420623, 0.9995235871707959241, 0.000000000000000000 ) ) ;
#14443 = ORIENTED_EDGE ( 'NONE', *, *, #15992, .F. ) ;
#14444 = ORIENTED_EDGE ( 'NONE', *, *, #12963, .F. ) ;
#14445 = CARTESIAN_POINT ( 'NONE',  ( 10.00000000000000000, -50.69000562871624993, -24.68609584167212745 ) ) ;
#14446 = ORIENTED_EDGE ( 'NONE', *, *, #5918, .F. ) ;
#14447 = CARTESIAN_POINT ( 'NONE',  ( 0.000000000000000000, -30.00000000000000000, 20.00000000000000000 ) ) ;
#14448 = EDGE_CURVE ( 'NONE', #72, #17369, #5970, .T. ) ;
#14449 = PRODUCT_DEFINITION_FORMATION_WITH_SPECIFIED_SOURCE ( 'ANY', '', #15750, .NOT_KNOWN. ) ;
#14450 = EDGE_CURVE ( 'NONE', #12264, #10921, #13891, .T. ) ;
#14451 = AXIS2_PLACEMENT_3D ( 'NONE', #15140, #13115, #14815 ) ;
#14452 = AXIS2_PLACEMENT_3D ( 'NONE', #13658, #5258, #2214 ) ;
#14453 = PRODUCT_DEFINITION ( 'UNKNOWN', '', #13841, #5787 ) ;
#14454 = CARTESIAN_POINT ( 'NONE',  ( 0.000000000000000000, -34.99999999999999289, 0.000000000000000000 ) ) ;
#14455 = ORIENTED_EDGE ( 'NONE', *, *, #4149, .T. ) ;
#14456 = ADVANCED_FACE ( 'NONE', ( #1268 ), #18499, .T. ) ;
#14457 = CIRCLE ( 'NONE', #796, 24.00000000002399148 ) ;
#14458 = ORIENTED_EDGE ( 'NONE', *, *, #14589, .T. ) ;
#14459 = DIRECTION ( 'NONE',  ( 0.000000000000000000, -1.000000000000000000, 0.000000000000000000 ) ) ;
#14460 = DIRECTION ( 'NONE',  ( -1.000000000000000000, 0.000000000000000000, -0.000000000000000000 ) ) ;
#14461 = DIRECTION ( 'NONE',  ( 0.000000000000000000, 0.000000000000000000, -1.000000000000000000 ) ) ;
#14462 = DIRECTION ( 'NONE',  ( 0.000000000000000000, 1.000000000000000000, -1.287488025362403787E-15 ) ) ;
#14463 = DIRECTION ( 'NONE',  ( 0.000000000000000000, 0.000000000000000000, -1.000000000000000000 ) ) ;
#14464 = EDGE_CURVE ( 'NONE', #2709, #13973, #18683, .T. ) ;
#14465 = DIRECTION ( 'NONE',  ( 0.000000000000000000, -0.3090169943749349613, -0.9510565162951576390 ) ) ;
#14466 = CARTESIAN_POINT ( 'NONE',  ( 10.00000000000000000, 0.000000000000000000, 0.000000000000000000 ) ) ;
#14467 = CIRCLE ( 'NONE', #10200, 56.24900000005625600 ) ;
#14468 = CARTESIAN_POINT ( 'NONE',  ( -0.6448876103708541807, -4.246476118072358474, -0.2256878752776773356 ) ) ;
#14469 = EDGE_LOOP ( 'NONE', ( #4926, #11022, #17886, #18630, #15098 ) ) ;
#14470 = CARTESIAN_POINT ( 'NONE',  ( -2.836893136758495970, -3.208949435745868328, -3.505054077164885484 ) ) ;
#14471 = EDGE_LOOP ( 'NONE', ( #1669, #10540, #181, #1993 ) ) ;
#14472 = DIRECTION ( 'NONE',  ( 0.000000000000000000, 0.000000000000000000, -1.000000000000000000 ) ) ;
#14473 = CARTESIAN_POINT ( 'NONE',  ( 0.000000000000000000, 0.000000000000000000, 4.000000000000000000 ) ) ;
#14474 = ADVANCED_FACE ( 'NONE', ( #2782, #13069 ), #10197, .T. ) ;
#14475 = EDGE_CURVE ( 'NONE', #3589, #2422, #14397, .T. ) ;
#14476 = ORIENTED_EDGE ( 'NONE', *, *, #15298, .F. ) ;
#14477 = AXIS2_PLACEMENT_3D ( 'NONE', #240, #13195, #3382 ) ;
#14478 =( GEOMETRIC_REPRESENTATION_CONTEXT ( 3 ) GLOBAL_UNCERTAINTY_ASSIGNED_CONTEXT ( ( #18333 ) ) GLOBAL_UNIT_ASSIGNED_CONTEXT ( ( #17749, #4420, #16143 ) ) REPRESENTATION_CONTEXT ( 'NONE', 'WORKASPACE' ) );
#14479 = AXIS2_PLACEMENT_3D ( 'NONE', #5742, #6005, #1451 ) ;
#14480 = EDGE_CURVE ( 'NONE', #3817, #9138, #15921, .T. ) ;
#14481 = VECTOR ( 'NONE', #5089, 1000.000000000000000 ) ;
#14482 = AXIS2_PLACEMENT_3D ( 'NONE', #3311, #1677, #11783 ) ;
#14483 = AXIS2_PLACEMENT_3D ( 'NONE', #11539, #13232, #17704 ) ;
#14484 = ADVANCED_FACE ( 'NONE', ( #5634 ), #2872, .T. ) ;
#14485 = ORIENTED_EDGE ( 'NONE', *, *, #3183, .F. ) ;
#14486 = DIRECTION ( 'NONE',  ( -1.000000000000000000, 0.000000000000000000, 0.000000000000000000 ) ) ;
#14487 = CARTESIAN_POINT ( 'NONE',  ( 2.500000000000000000, 0.000000000000000000, 2.041999999999999815 ) ) ;
#14488 = ORIENTED_EDGE ( 'NONE', *, *, #9183, .F. ) ;
#14489 = FACE_BOUND ( 'NONE', #3302, .T. ) ;
#14490 = DIRECTION ( 'NONE',  ( -0.000000000000000000, 1.000000000000000000, -0.000000000000000000 ) ) ;
#14491 = LINE ( 'NONE', #1545, #10085 ) ;
#14492 = DIRECTION ( 'NONE',  ( -1.000000000000000000, -0.000000000000000000, -0.000000000000000000 ) ) ;
#14493 = ORIENTED_EDGE ( 'NONE', *, *, #1875, .T. ) ;
#14494 = FACE_OUTER_BOUND ( 'NONE', #12488, .T. ) ;
#14495 = VECTOR ( 'NONE', #14574, 1000.000000000000000 ) ;
#14496 = ORIENTED_EDGE ( 'NONE', *, *, #11272, .F. ) ;
#14497 = AXIS2_PLACEMENT_3D ( 'NONE', #963, #8382, #6959 ) ;
#14498 = FACE_OUTER_BOUND ( 'NONE', #354, .T. ) ;
#14499 = DIRECTION ( 'NONE',  ( -1.000000000000000000, 0.000000000000000000, -0.000000000000000000 ) ) ;
#14500 = ORIENTED_EDGE ( 'NONE', *, *, #14415, .F. ) ;
#14501 = CIRCLE ( 'NONE', #15714, 12.00000000001200640 ) ;
#14502 = CIRCLE ( 'NONE', #16950, 24.00000000002400569 ) ;
#14503 = B_SPLINE_CURVE_WITH_KNOTS ( 'NONE', 3,
 ( #7916, #12291, #18292, #16687, #781, #6582 ),
 .UNSPECIFIED., .F., .F.,
 ( 4, 2, 4 ),
 ( 0.003358874760055550156, 0.004541967308452096383, 0.005725059856848641743 ),
 .UNSPECIFIED. ) ;
#14504 = APPLICATION_PROTOCOL_DEFINITION ( 'draft international standard', 'automotive_design', 1998, #11199 ) ;
#14505 = ORIENTED_EDGE ( 'NONE', *, *, #6072, .F. ) ;
#14506 = AXIS2_PLACEMENT_3D ( 'NONE', #14112, #9743, #15902 ) ;
#14507 = ADVANCED_FACE ( 'NONE', ( #17360 ), #8498, .T. ) ;
#14508 = AXIS2_PLACEMENT_3D ( 'NONE', #17612, #11887, #13052 ) ;
#14509 = CARTESIAN_POINT ( 'NONE',  ( -90.38553543446691663, 1.000000000000018208, -4.784491867360616268 ) ) ;
#14510 = CARTESIAN_POINT ( 'NONE',  ( 4.154306624730864428, 2.398490048084778170, -3.721999068284300272 ) ) ;
#14511 = AXIS2_PLACEMENT_3D ( 'NONE', #413, #2123, #13655 ) ;
#14512 = CARTESIAN_POINT ( 'NONE',  ( -11.25000000000000355, 3.073863465859856794E-15, -25.10000000000000142 ) ) ;
#14513 = CARTESIAN_POINT ( 'NONE',  ( 10.00000000000000000, 26.20671763660628528, -1.489278925039611901 ) ) ;
#14514 = DIRECTION ( 'NONE',  ( -0.000000000000000000, 1.000000000000000000, -0.000000000000000000 ) ) ;
#14515 = ORIENTED_EDGE ( 'NONE', *, *, #10503, .F. ) ;
#14516 = CARTESIAN_POINT ( 'NONE',  ( 0.000000000000000000, -62.87238730325618263, -4.007856633824049553 ) ) ;
#14517 = LINE ( 'NONE', #1298, #11659 ) ;
#14518 = LINE ( 'NONE', #4422, #2439 ) ;
#14519 = AXIS2_PLACEMENT_3D ( 'NONE', #3417, #3225, #18070 ) ;
#14520 = ORIENTED_EDGE ( 'NONE', *, *, #14011, .F. ) ;
#14521 = ORIENTED_EDGE ( 'NONE', *, *, #6563, .F. ) ;
#14522 = DIRECTION ( 'NONE',  ( 1.000000000000000000, 0.000000000000000000, 0.000000000000000000 ) ) ;
#14523 = SHAPE_REPRESENTATION_RELATIONSHIP ( 'NONE' , 'NONE' ,  #2517, #17412 ) ;
#14524 = AXIS2_PLACEMENT_3D ( 'NONE', #11463, #10126, #2701 ) ;
#14525 = ORIENTED_EDGE ( 'NONE', *, *, #17636, .T. ) ;
#14526 = AXIS2_PLACEMENT_3D ( 'NONE', #17481, #15874, #70 ) ;
#14527 = VECTOR ( 'NONE', #6482, 1000.000000000000000 ) ;
#14528 = PRODUCT_DEFINITION_SHAPE ( 'NONE', 'NONE',  #18845 ) ;
#14529 = EDGE_CURVE ( 'NONE', #3994, #15653, #11755, .T. ) ;
#14530 = DIRECTION ( 'NONE',  ( -1.000000000000000000, -0.000000000000000000, -0.000000000000000000 ) ) ;
#14531 = CARTESIAN_POINT ( 'NONE',  ( 0.000000000000000000, 0.000000000000000000, -4.000000000000000000 ) ) ;
#14532 = CARTESIAN_POINT ( 'NONE',  ( 10.00000000000000000, 0.000000000000000000, 0.000000000000000000 ) ) ;
#14533 = ORIENTED_EDGE ( 'NONE', *, *, #17230, .T. ) ;
#14534 = DIRECTION ( 'NONE',  ( -1.000000000000000000, 0.000000000000000000, 0.000000000000000000 ) ) ;
#14535 = AXIS2_PLACEMENT_3D ( 'NONE', #12993, #12899, #10034 ) ;
#14536 = AXIS2_PLACEMENT_3D ( 'NONE', #3459, #323, #18019 ) ;
#14537 = ORIENTED_EDGE ( 'NONE', *, *, #10607, .F. ) ;
#14538 = PRODUCT_DEFINITION_CONTEXT ( 'detailed design', #14979, 'design' ) ;
#14539 = AXIS2_PLACEMENT_3D ( 'NONE', #12099, #10757, #13357 ) ;
#14540 = DIRECTION ( 'NONE',  ( 0.000000000000000000, 0.000000000000000000, 1.000000000000000000 ) ) ;
#14541 = ORIENTED_EDGE ( 'NONE', *, *, #6205, .F. ) ;
#14542 = ORIENTED_EDGE ( 'NONE', *, *, #2828, .T. ) ;
#14543 = CARTESIAN_POINT ( 'NONE',  ( 10.00000000000000000, 0.000000000000000000, 0.000000000000000000 ) ) ;
#14544 = CARTESIAN_POINT ( 'NONE',  ( -97.50000000009001155, -13.00000000000001599, -1.691355389077386325E-15 ) ) ;
#14545 = ORIENTED_EDGE ( 'NONE', *, *, #15830, .T. ) ;
#14546 = ORIENTED_EDGE ( 'NONE', *, *, #16547, .T. ) ;
#14547 = EDGE_CURVE ( 'NONE', #3169, #16256, #16619, .T. ) ;
#14548 = CARTESIAN_POINT ( 'NONE',  ( 10.00000000000000000, 1.489278925039883239, -26.20671763660627107 ) ) ;
#14549 = ORIENTED_EDGE ( 'NONE', *, *, #1898, .F. ) ;
#14550 = DIRECTION ( 'NONE',  ( 1.000000000000000000, 0.000000000000000000, 0.000000000000000000 ) ) ;
#14551 = VECTOR ( 'NONE', #8614, 1000.000000000000000 ) ;
#14552 = AXIS2_PLACEMENT_3D ( 'NONE', #4479, #469, #17798 ) ;
#14553 = EDGE_CURVE ( 'NONE', #17667, #4599, #17443, .T. ) ;
#14554 = AXIS2_PLACEMENT_3D ( 'NONE', #8118, #7924, #9637 ) ;
#14555 = AXIS2_PLACEMENT_3D ( 'NONE', #11223, #13793, #755 ) ;
#14556 = CARTESIAN_POINT ( 'NONE',  ( 0.000000000000000000, 1.305124410222461284, -2.000000000000000000 ) ) ;
#14557 = EDGE_LOOP ( 'NONE', ( #12004, #3455, #7741, #639 ) ) ;
#14558 = CIRCLE ( 'NONE', #9380, 2.649999999999999467 ) ;
#14559 = ORIENTED_EDGE ( 'NONE', *, *, #780, .T. ) ;
#14560 = DIRECTION ( 'NONE',  ( 0.000000000000000000, 0.000000000000000000, -1.000000000000000000 ) ) ;
#14561 = DIRECTION ( 'NONE',  ( 1.000000000000000000, 0.000000000000000000, 0.000000000000000000 ) ) ;
#14562 = CYLINDRICAL_SURFACE ( 'NONE', #14519, 6.080745460913608902 ) ;
#14563 = ORIENTED_EDGE ( 'NONE', *, *, #10856, .T. ) ;
#14564 = CYLINDRICAL_SURFACE ( 'NONE', #12069, 4.799999999999998934 ) ;
#14565 = AXIS2_PLACEMENT_3D ( 'NONE', #16260, #172, #13132 ) ;
#14566 = EDGE_CURVE ( 'NONE', #8186, #3193, #5055, .T. ) ;
#14567 = CARTESIAN_POINT ( 'NONE',  ( 5.000000000000000888, 0.000000000000000000, 0.000000000000000000 ) ) ;
#14568 = DIRECTION ( 'NONE',  ( 0.000000000000000000, -0.7071067811865535679, 0.7071067811865413555 ) ) ;
#14569 = AXIS2_PLACEMENT_3D ( 'NONE', #1051, #17424, #11617 ) ;
#14570 = FACE_BOUND ( 'NONE', #348, .T. ) ;
#14571 = ORIENTED_EDGE ( 'NONE', *, *, #18158, .T. ) ;
#14572 = CIRCLE ( 'NONE', #6362, 24.00000000002399503 ) ;
#14573 = CARTESIAN_POINT ( 'NONE',  ( 10.00000000000000000, -29.03656532225551601, -15.68049343256028294 ) ) ;
#14574 = DIRECTION ( 'NONE',  ( -1.000000000000000000, 0.000000000000000000, 0.000000000000000000 ) ) ;
#14575 = ORIENTED_EDGE ( 'NONE', *, *, #12321, .T. ) ;
#14576 = DIRECTION ( 'NONE',  ( 0.000000000000000000, 0.000000000000000000, 1.000000000000000000 ) ) ;
#14577 = CARTESIAN_POINT ( 'NONE',  ( 0.000000000000000000, 0.000000000000000000, 0.000000000000000000 ) ) ;
#14578 = ITEM_DEFINED_TRANSFORMATION ( 'NONE', 'NONE', #18095,  #8017 ) ;
#14579 = AXIS2_PLACEMENT_3D ( 'NONE', #10397, #6295, #9057 ) ;
#14580 = AXIS2_PLACEMENT_3D ( 'NONE', #2445, #14063, #1023 ) ;
#14581 = ORIENTED_EDGE ( 'NONE', *, *, #15047, .F. ) ;
#14582 = CARTESIAN_POINT ( 'NONE',  ( 10.00000000000000000, 18.64666490672447097, -53.06836994729213330 ) ) ;
#14583 = DIRECTION ( 'NONE',  ( -1.000000000000000000, 0.000000000000000000, 0.000000000000000000 ) ) ;
#14584 = ORIENTED_EDGE ( 'NONE', *, *, #11210, .T. ) ;
#14585 =( NAMED_UNIT ( * ) SI_UNIT ( $, .STERADIAN. ) SOLID_ANGLE_UNIT ( ) );
#14586 = EDGE_CURVE ( 'NONE', #6251, #5299, #5460, .T. ) ;
#14587 = DIRECTION ( 'NONE',  ( 0.000000000000000000, -0.000000000000000000, 1.000000000000000000 ) ) ;
#14588 = EDGE_CURVE ( 'NONE', #10272, #16476, #2582, .T. ) ;
#14589 = EDGE_CURVE ( 'NONE', #3492, #18225, #18754, .T. ) ;
#14590 = LINE ( 'NONE', #11554, #15762 ) ;
#14591 = AXIS2_PLACEMENT_3D ( 'NONE', #14663, #4749, #13149 ) ;
#14592 = DIRECTION ( 'NONE',  ( -0.000000000000000000, 1.000000000000000000, -0.000000000000000000 ) ) ;
#14593 = DIRECTION ( 'NONE',  ( -1.000000000000000000, -0.000000000000000000, 0.000000000000000000 ) ) ;
#14594 = ORIENTED_EDGE ( 'NONE', *, *, #10662, .F. ) ;
#14595 = DIRECTION ( 'NONE',  ( 1.000000000000000000, -0.000000000000000000, -0.000000000000000000 ) ) ;
#14596 = ORIENTED_EDGE ( 'NONE', *, *, #7498, .T. ) ;
#14597 = ADVANCED_FACE ( 'NONE', ( #11444 ), #14212, .T. ) ;
#14598 = DIRECTION ( 'NONE',  ( -1.000000000000000000, -0.000000000000000000, 0.000000000000000000 ) ) ;
#14599 = DIRECTION ( 'NONE',  ( 1.000000000000000000, 0.000000000000000000, 0.000000000000000000 ) ) ;
#14600 = ORIENTED_EDGE ( 'NONE', *, *, #6782, .F. ) ;
#14601 = SHAPE_DEFINITION_REPRESENTATION ( #12862, #13460 ) ;
#14602 = EDGE_CURVE ( 'NONE', #9474, #752, #12786, .T. ) ;
#14603 = ORIENTED_EDGE ( 'NONE', *, *, #9564, .T. ) ;
#14604 = ADVANCED_FACE ( 'NONE', ( #7062 ), #12885, .T. ) ;
#14605 = CIRCLE ( 'NONE', #13698, 2.649999999999999467 ) ;
#14606 = ORIENTED_EDGE ( 'NONE', *, *, #12493, .F. ) ;
#14607 = FACE_BOUND ( 'NONE', #15323, .T. ) ;
#14608 = CARTESIAN_POINT ( 'NONE',  ( 4.000000000000000000, 2.309401076758497151, -3.433295621305379353 ) ) ;
#14609 = FACE_OUTER_BOUND ( 'NONE', #2292, .T. ) ;
#14610 = CARTESIAN_POINT ( 'NONE',  ( 0.000000000000000000, 53.22058882792246237, -33.71303790549217183 ) ) ;
#14611 = EDGE_CURVE ( 'NONE', #845, #168, #5007, .T. ) ;
#14612 = CARTESIAN_POINT ( 'NONE',  ( 10.00000000000000000, -32.11449294037235092, 54.20017844242499905 ) ) ;
#14613 = DIRECTION ( 'NONE',  ( 0.000000000000000000, -0.5000000000000009992, -0.8660254037844380415 ) ) ;
#14614 = CARTESIAN_POINT ( 'NONE',  ( 0.000000000000000000, -7.478235706489372525, 55.74967257055880054 ) ) ;
#14615 = ORIENTED_EDGE ( 'NONE', *, *, #14566, .T. ) ;
#14616 = PRESENTATION_STYLE_ASSIGNMENT (( #16233 ) ) ;
#14617 = CARTESIAN_POINT ( 'NONE',  ( 13.90576474687299680, 0.000000000000000000, 40.14754323328178742 ) ) ;
#14618 = FACE_OUTER_BOUND ( 'NONE', #6129, .T. ) ;
#14619 = ORIENTED_EDGE ( 'NONE', *, *, #8999, .F. ) ;
#14620 = ORIENTED_EDGE ( 'NONE', *, *, #2007, .T. ) ;
#14621 =( REPRESENTATION_RELATIONSHIP ('NONE','NONE', #11014, #16765 ) REPRESENTATION_RELATIONSHIP_WITH_TRANSFORMATION ( #8213 )SHAPE_REPRESENTATION_RELATIONSHIP( ) );
#14622 = EDGE_CURVE ( 'NONE', #4981, #4644, #840, .T. ) ;
#14623 = LINE ( 'NONE', #4066, #16597 ) ;
#14624 = AXIS2_PLACEMENT_3D ( 'NONE', #6495, #6211, #15075 ) ;
#14625 = DIRECTION ( 'NONE',  ( 0.000000000000000000, 0.000000000000000000, 1.000000000000000000 ) ) ;
#14626 = EDGE_LOOP ( 'NONE', ( #4876, #426, #18230, #13551 ) ) ;
#14627 = CARTESIAN_POINT ( 'NONE',  ( 5.032868406504333869, -28.36021363089093938, 0.000000000000000000 ) ) ;
#14628 = CARTESIAN_POINT ( 'NONE',  ( 0.000000000000000000, -26.50000000000000000, -41.00000000000000000 ) ) ;
#14629 = DIRECTION ( 'NONE',  ( 0.000000000000000000, -1.287488025362403787E-15, -1.000000000000000000 ) ) ;
#14630 = ORIENTED_EDGE ( 'NONE', *, *, #9888, .T. ) ;
#14632 = CIRCLE ( 'NONE', #16149, 63.00000000006298961 ) ;
#14631 = DIRECTION ( 'NONE',  ( 1.000000000000000000, 0.000000000000000000, 0.000000000000000000 ) ) ;
#14633 = EDGE_LOOP ( 'NONE', ( #13006, #14760, #5121, #14089 ) ) ;
#14634 = CARTESIAN_POINT ( 'NONE',  ( -36.40576474687247099, 10.00000000000000000, 26.45033635316149301 ) ) ;
#14635 = ORIENTED_EDGE ( 'NONE', *, *, #4240, .T. ) ;
#14636 = EDGE_LOOP ( 'NONE', ( #17411, #18731 ) ) ;
#14637 = LINE ( 'NONE', #7395, #15395 ) ;
#14638 = CARTESIAN_POINT ( 'NONE',  ( 1.747541505913279281, -3.837784562140273081, -3.503702292528912299 ) ) ;
#14639 = ORIENTED_EDGE ( 'NONE', *, *, #12493, .T. ) ;
#14640 = ORIENTED_EDGE ( 'NONE', *, *, #2665, .F. ) ;
#14641 = EDGE_CURVE ( 'NONE', #12365, #18659, #12255, .T. ) ;
#14642 = DIRECTION ( 'NONE',  ( -1.000000000000000000, 0.000000000000000000, -0.000000000000000000 ) ) ;
#14643 = PRESENTATION_STYLE_ASSIGNMENT (( #14833 ) ) ;
#14644 = ORIENTED_EDGE ( 'NONE', *, *, #6030, .T. ) ;
#14645 = FACE_OUTER_BOUND ( 'NONE', #10481, .T. ) ;
#14646 = CIRCLE ( 'NONE', #5523, 56.24900000005625600 ) ;
#14647 = AXIS2_PLACEMENT_3D ( 'NONE', #16721, #12228, #9656 ) ;
#14648 = AXIS2_PLACEMENT_3D ( 'NONE', #14454, #17336, #1414 ) ;
#14649 = CYLINDRICAL_SURFACE ( 'NONE', #3725, 27.00000000000000355 ) ;
#14650 = ORIENTED_EDGE ( 'NONE', *, *, #12168, .F. ) ;
#14651 = EDGE_CURVE ( 'NONE', #3993, #13575, #13905, .T. ) ;
#14652 = ORIENTED_EDGE ( 'NONE', *, *, #5143, .T. ) ;
#14653 = DIRECTION ( 'NONE',  ( 0.000000000000000000, 0.3090169943749411785, 0.9510565162951556406 ) ) ;
#14654 = PLANE ( 'NONE',  #7142 ) ;
#14655 = DIRECTION ( 'NONE',  ( -1.000000000000000000, 0.000000000000000000, 0.000000000000000000 ) ) ;
#14656 = ORIENTED_EDGE ( 'NONE', *, *, #4202, .T. ) ;
#14657 = FACE_OUTER_BOUND ( 'NONE', #7070, .T. ) ;
#14658 = EDGE_CURVE ( 'NONE', #13064, #15277, #1624, .T. ) ;
#14659 = CARTESIAN_POINT ( 'NONE',  ( -117.1020693116508085, -34.99999999999999289, 22.34080595179777262 ) ) ;
#14660 = DIRECTION ( 'NONE',  ( -0.000000000000000000, -1.000000000000000000, -0.000000000000000000 ) ) ;
#14661 = DIRECTION ( 'NONE',  ( 0.000000000000000000, 1.000000000000000000, 0.000000000000000000 ) ) ;
#14662 = ORIENTED_EDGE ( 'NONE', *, *, #8659, .F. ) ;
#14663 = CARTESIAN_POINT ( 'NONE',  ( -90.00000000009001155, -34.99999999999999289, -1.301042606982603940E-15 ) ) ;
#14664 = CIRCLE ( 'NONE', #17110, 27.00000000000000355 ) ;
#14665 = EDGE_CURVE ( 'NONE', #6377, #3113, #6539, .T. ) ;
#14666 = ORIENTED_EDGE ( 'NONE', *, *, #66, .F. ) ;
#14667 = DIRECTION ( 'NONE',  ( 0.000000000000000000, 0.000000000000000000, 1.000000000000000000 ) ) ;
#14668 = CARTESIAN_POINT ( 'NONE',  ( 10.00000000000000000, 24.79895094899259789, -13.40641754777674421 ) ) ;
#14669 = EDGE_LOOP ( 'NONE', ( #2742, #15453, #17445, #14053 ) ) ;
#14671 = DIRECTION ( 'NONE',  ( 0.000000000000000000, 0.8660254037844380415, -0.5000000000000009992 ) ) ;
#14670 = CIRCLE ( 'NONE', #4641, 4.349594641156947716 ) ;
#14672 = CARTESIAN_POINT ( 'NONE',  ( 0.000000000000000000, 55.83748330407408389, 16.18620087215052195 ) ) ;
#14673 = AXIS2_PLACEMENT_3D ( 'NONE', #8969, #15080, #2032 ) ;
#14674 = ORIENTED_EDGE ( 'NONE', *, *, #2166, .T. ) ;
#14675 = DIRECTION ( 'NONE',  ( 0.000000000000000000, 0.000000000000000000, 1.000000000000000000 ) ) ;
#14676 = CYLINDRICAL_SURFACE ( 'NONE', #16925, 33.00000000003299760 ) ;
#14677 = LINE ( 'NONE', #7431, #14527 ) ;
#14678 = DIRECTION ( 'NONE',  ( 0.000000000000000000, 0.000000000000000000, 1.000000000000000000 ) ) ;
#14679 = LINE ( 'NONE', #13253, #3521 ) ;
#14680 = VERTEX_POINT ( 'NONE', #11903 ) ;
#14681 = CARTESIAN_POINT ( 'NONE',  ( 2.500000000000000000, 0.000000000000000000, 0.000000000000000000 ) ) ;
#14682 = ORIENTED_EDGE ( 'NONE', *, *, #8088, .F. ) ;
#14683 =( LENGTH_UNIT ( ) NAMED_UNIT ( * ) SI_UNIT ( .MILLI., .METRE. ) );
#14684 = DIRECTION ( 'NONE',  ( 0.000000000000000000, -0.000000000000000000, 1.000000000000000000 ) ) ;
#14685 = ORIENTED_EDGE ( 'NONE', *, *, #2841, .T. ) ;
#14686 = APPLICATION_PROTOCOL_DEFINITION ( 'draft international standard', 'automotive_design', 1998, #11448 ) ;
#14687 = CIRCLE ( 'NONE', #11951, 63.00000000006298961 ) ;
#14688 = ORIENTED_EDGE ( 'NONE', *, *, #7494, .T. ) ;
#14689 = AXIS2_PLACEMENT_3D ( 'NONE', #888, #6686, #2488 ) ;
#14690 = ADVANCED_FACE ( 'NONE', ( #1537 ), #5070, .T. ) ;
#14691 = EDGE_CURVE ( 'NONE', #13493, #6730, #5979, .T. ) ;
#14692 = CARTESIAN_POINT ( 'NONE',  ( 0.000000000000000000, -61.03368945066424800, -15.61693798565561409 ) ) ;
#14693 = EDGE_CURVE ( 'NONE', #1353, #3828, #6900, .T. ) ;
#14694 = DIRECTION ( 'NONE',  ( -0.000000000000000000, 1.000000000000000000, -0.000000000000000000 ) ) ;
#14695 = DIRECTION ( 'NONE',  ( 0.000000000000000000, 0.000000000000000000, 1.000000000000000000 ) ) ;
#14696 = DIRECTION ( 'NONE',  ( 0.000000000000000000, 0.000000000000000000, 1.000000000000000000 ) ) ;
#14697 = EDGE_CURVE ( 'NONE', #906, #9845, #4182, .T. ) ;
#14698 = CIRCLE ( 'NONE', #8009, 24.00000000002399858 ) ;
#14699 = CARTESIAN_POINT ( 'NONE',  ( -0.3865131578947368918, -23.49682122285426189, -2.000000000000000000 ) ) ;
#14700 = DIRECTION ( 'NONE',  ( -1.000000000000000000, -0.000000000000000000, -0.000000000000000000 ) ) ;
#14701 = DIRECTION ( 'NONE',  ( 1.000000000000000000, 0.000000000000000000, 2.220446049250313081E-16 ) ) ;
#14702 = EDGE_LOOP ( 'NONE', ( #18359, #8630, #3343 ) ) ;
#14703 = SURFACE_STYLE_FILL_AREA ( #7367 ) ;
#14704 = EDGE_CURVE ( 'NONE', #14729, #15974, #3063, .T. ) ;
#14705 = DIRECTION ( 'NONE',  ( 0.000000000000000000, -0.8910065241883722287, 0.4539904997395383113 ) ) ;
#14706 = LINE ( 'NONE', #519, #9972 ) ;
#14707 = ORIENTED_EDGE ( 'NONE', *, *, #8679, .T. ) ;
#14708 = ORIENTED_EDGE ( 'NONE', *, *, #16702, .F. ) ;
#14709 = CARTESIAN_POINT ( 'NONE',  ( -12.50000000000000533, 0.000000000000000000, -28.00000000000000355 ) ) ;
#14710 = DIRECTION ( 'NONE',  ( 0.000000000000000000, 0.000000000000000000, 1.000000000000000000 ) ) ;
#14711 = CARTESIAN_POINT ( 'NONE',  ( 5.200000000000002842, 0.000000000000000000, 0.000000000000000000 ) ) ;
#14712 = VERTEX_POINT ( 'NONE', #16011 ) ;
#14713 = ADVANCED_FACE ( 'NONE', ( #13351 ), #10466, .T. ) ;
#14714 = STYLED_ITEM ( 'NONE', ( #682 ), #9198 ) ;
#14715 = EDGE_CURVE ( 'NONE', #11197, #12068, #5699, .T. ) ;
#14716 = CARTESIAN_POINT ( 'NONE',  ( -90.00000000009001155, 2.081668171172168513E-14, -5.000000000000005329 ) ) ;
#14717 = ADVANCED_FACE ( 'NONE', ( #3246 ), #16029, .T. ) ;
#14718 = CARTESIAN_POINT ( 'NONE',  ( 1.243802165048773611, -3.900692638707475624, -3.223146290109810241 ) ) ;
#14719 = CARTESIAN_POINT ( 'NONE',  ( 5.000000000000000000, -4.381479206522763015, -32.70783759231090926 ) ) ;
#14720 = EDGE_CURVE ( 'NONE', #10905, #10374, #1139, .T. ) ;
#14721 = ORIENTED_EDGE ( 'NONE', *, *, #4000, .T. ) ;
#14722 = DIRECTION ( 'NONE',  ( 0.000000000000000000, 0.000000000000000000, 1.000000000000000000 ) ) ;
#14723 = ORIENTED_EDGE ( 'NONE', *, *, #5887, .T. ) ;
#14724 = DIRECTION ( 'NONE',  ( -1.000000000000000000, -0.000000000000000000, -0.000000000000000000 ) ) ;
#14725 = ORIENTED_EDGE ( 'NONE', *, *, #8492, .F. ) ;
#14726 = APPLICATION_CONTEXT ( 'automotive_design' ) ;
#14727 = FACE_OUTER_BOUND ( 'NONE', #15811, .T. ) ;
#14728 = FACE_OUTER_BOUND ( 'NONE', #18484, .T. ) ;
#14729 = VERTEX_POINT ( 'NONE', #1815 ) ;
#14730 = ORIENTED_EDGE ( 'NONE', *, *, #11237, .T. ) ;
#14731 = CYLINDRICAL_SURFACE ( 'NONE', #7172, 5.000000000000004441 ) ;
#14732 = ORIENTED_EDGE ( 'NONE', *, *, #14388, .F. ) ;
#14733 = DIRECTION ( 'NONE',  ( 0.000000000000000000, 0.000000000000000000, -1.000000000000000000 ) ) ;
#14734 =( GEOMETRIC_REPRESENTATION_CONTEXT ( 3 ) GLOBAL_UNCERTAINTY_ASSIGNED_CONTEXT ( ( #6149 ) ) GLOBAL_UNIT_ASSIGNED_CONTEXT ( ( #9900, #11589, #17393 ) ) REPRESENTATION_CONTEXT ( 'NONE', 'WORKASPACE' ) );
#14735 = DIRECTION ( 'NONE',  ( -1.000000000000000000, -0.000000000000000000, -0.000000000000000000 ) ) ;
#14736 = CIRCLE ( 'NONE', #17478, 40.00000000000000000 ) ;
#14737 = EDGE_CURVE ( 'NONE', #16747, #2351, #10549, .T. ) ;
#14738 = ORIENTED_EDGE ( 'NONE', *, *, #4470, .T. ) ;
#14739 = ORIENTED_EDGE ( 'NONE', *, *, #1231, .F. ) ;
#14740 = CYLINDRICAL_SURFACE ( 'NONE', #18780, 56.24900000005625600 ) ;
#14741 = CARTESIAN_POINT ( 'NONE',  ( 5.000000000000000000, 5.876895005583342879, -62.72529079327799906 ) ) ;
#14742 = DIRECTION ( 'NONE',  ( -1.000000000000000000, 0.000000000000000000, 0.000000000000000000 ) ) ;
#14743 = ORIENTED_EDGE ( 'NONE', *, *, #2954, .F. ) ;
#14744 = CARTESIAN_POINT ( 'NONE',  ( -4.211405944401398038, -2.460460786169389902, -3.751298493805494072 ) ) ;
#14745 = DIRECTION ( 'NONE',  ( 0.000000000000000000, -0.8090169943749402348, -0.5877852522924831291 ) ) ;
#14746 = FACE_OUTER_BOUND ( 'NONE', #9653, .T. ) ;
#14747 = CARTESIAN_POINT ( 'NONE',  ( 32.50000000000000000, -30.00000000000000000, 3.680389326632394941E-13 ) ) ;
#14748 = VERTEX_POINT ( 'NONE', #115 ) ;
#14749 = DIRECTION ( 'NONE',  ( -1.000000000000000000, 0.000000000000000000, 0.000000000000000000 ) ) ;
#14750 = CYLINDRICAL_SURFACE ( 'NONE', #6281, 23.50000000000000355 ) ;
#14751 = PRODUCT_DEFINITION_FORMATION_WITH_SPECIFIED_SOURCE ( 'ANY', '', #15589, .NOT_KNOWN. ) ;
#14752 = ORIENTED_EDGE ( 'NONE', *, *, #3683, .F. ) ;
#14753 = DIRECTION ( 'NONE',  ( 1.000000000000000000, 0.000000000000000000, 0.000000000000000000 ) ) ;
#14754 = PLANE ( 'NONE',  #711 ) ;
#14755 = AXIS2_PLACEMENT_3D ( 'NONE', #2075, #12254, #7881 ) ;
#14756 = VECTOR ( 'NONE', #14319, 1000.000000000000114 ) ;
#14757 = ADVANCED_FACE ( 'NONE', ( #10383 ), #18156, .T. ) ;
#14758 = EDGE_CURVE ( 'NONE', #15167, #445, #15122, .T. ) ;
#14759 = AXIS2_PLACEMENT_3D ( 'NONE', #1984, #14642, #17414 ) ;
#14760 = ORIENTED_EDGE ( 'NONE', *, *, #10751, .F. ) ;
#14761 = DIRECTION ( 'NONE',  ( -1.000000000000000000, -0.000000000000000000, -0.000000000000000000 ) ) ;
#14762 = CYLINDRICAL_SURFACE ( 'NONE', #14023, 0.7499999999999997780 ) ;
#14763 = VECTOR ( 'NONE', #10919, 1000.000000000000000 ) ;
#14764 = VERTEX_POINT ( 'NONE', #6734 ) ;
#14765 = AXIS2_PLACEMENT_3D ( 'NONE', #9524, #12102, #17918 ) ;
#14766 = DIRECTION ( 'NONE',  ( 0.000000000000000000, 0.000000000000000000, -1.000000000000000000 ) ) ;
#14767 = CARTESIAN_POINT ( 'NONE',  ( 10.00000000000000178, 0.000000000000000000, 5.000000000000000000 ) ) ;
#14768 = DIRECTION ( 'NONE',  ( -0.000000000000000000, 1.000000000000000000, -0.000000000000000000 ) ) ;
#14769 = DIRECTION ( 'NONE',  ( -1.000000000000000000, -0.000000000000000000, 0.000000000000000000 ) ) ;
#14770 = ORIENTED_EDGE ( 'NONE', *, *, #1787, .T. ) ;
#14771 = DIRECTION ( 'NONE',  ( -1.000000000000000000, -0.000000000000000000, -0.000000000000000000 ) ) ;
#14772 = ORIENTED_EDGE ( 'NONE', *, *, #2971, .T. ) ;
#14773 = CARTESIAN_POINT ( 'NONE',  ( -0.6666666666666651864, 4.233901974057260098, -3.300726591567081147 ) ) ;
#14774 = ORIENTED_EDGE ( 'NONE', *, *, #4757, .F. ) ;
#14775 = AXIS2_PLACEMENT_3D ( 'NONE', #12916, #14342, #14522 ) ;
#14776 = EDGE_CURVE ( 'NONE', #5713, #11318, #5398, .T. ) ;
#14777 = ORIENTED_EDGE ( 'NONE', *, *, #12831, .T. ) ;
#14778 = CIRCLE ( 'NONE', #11744, 4.000000000000000000 ) ;
#14779 = CIRCLE ( 'NONE', #8417, 56.24900000005626310 ) ;
#14780 = EDGE_CURVE ( 'NONE', #16544, #3711, #9949, .T. ) ;
#14781 = EDGE_LOOP ( 'NONE', ( #1952, #13875, #17951, #16422 ) ) ;
#14782 = VERTEX_POINT ( 'NONE', #17036 ) ;
#14783 = CARTESIAN_POINT ( 'NONE',  ( -10.00000000000000000, 0.000000000000000000, 0.000000000000000000 ) ) ;
#14784 = DIRECTION ( 'NONE',  ( 0.000000000000000000, 0.000000000000000000, 1.000000000000000000 ) ) ;
#14785 = AXIS2_PLACEMENT_3D ( 'NONE', #5565, #14231, #12707 ) ;
#14786 = PRESENTATION_LAYER_ASSIGNMENT (  '', '', ( #18751 ) ) ;
#14787 = DIRECTION ( 'NONE',  ( -1.000000000000000000, 0.000000000000000000, 0.000000000000000000 ) ) ;
#14788 = CARTESIAN_POINT ( 'NONE',  ( -26.29305231718568336, -34.99999999999999289, -19.10302069950552095 ) ) ;
#14789 = CIRCLE ( 'NONE', #1121, 2.649999999999992806 ) ;
#14790 = CARTESIAN_POINT ( 'NONE',  ( 10.00000000000000000, 7.813799127873274131, 55.83748330407410521 ) ) ;
#14791 = FACE_OUTER_BOUND ( 'NONE', #10979, .T. ) ;
#14792 = AXIS2_PLACEMENT_3D ( 'NONE', #5251, #6405, #12209 ) ;
#14793 = CARTESIAN_POINT ( 'NONE',  ( -90.00000000009001155, -30.00000000000000000, -10.00000000000001066 ) ) ;
#14794 = AXIS2_PLACEMENT_3D ( 'NONE', #3490, #257, #543 ) ;
#14795 = CARTESIAN_POINT ( 'NONE',  ( -90.40196296004810961, -14.11572627500821042, 6.951864913735147589 ) ) ;
#14796 = ORIENTED_EDGE ( 'NONE', *, *, #13934, .F. ) ;
#14797 = EDGE_CURVE ( 'NONE', #4490, #11098, #3980, .T. ) ;
#14798 = EDGE_CURVE ( 'NONE', #2015, #19, #1730, .T. ) ;
#14799 = CARTESIAN_POINT ( 'NONE',  ( 10.00000000000000000, -48.50907078259410099, 40.19788616105592638 ) ) ;
#14800 = DIRECTION ( 'NONE',  ( 0.000000000000000000, 0.000000000000000000, 1.000000000000000000 ) ) ;
#14801 = CARTESIAN_POINT ( 'NONE',  ( 2.500000000000000000, 2.357898499370432166, -2.385244779468109755E-15 ) ) ;
#14802 = ORIENTED_EDGE ( 'NONE', *, *, #4089, .T. ) ;
#14803 = VERTEX_POINT ( 'NONE', #3696 ) ;
#14804 = CARTESIAN_POINT ( 'NONE',  ( 10.00000000000000000, -45.00825343885045271, 33.95787273855228960 ) ) ;
#14805 = CARTESIAN_POINT ( 'NONE',  ( -36.40576474687271258, 15.00000000000001599, -26.45033635316118747 ) ) ;
#14806 = PRODUCT_RELATED_PRODUCT_CATEGORY ( 'part', '', ( #2666 ) ) ;
#14807 = LINE ( 'NONE', #2321, #16646 ) ;
#14808 = ORIENTED_EDGE ( 'NONE', *, *, #11792, .T. ) ;
#14809 = AXIS2_PLACEMENT_3D ( 'NONE', #18190, #5438, #15329 ) ;
#14810 = CIRCLE ( 'NONE', #7454, 33.00000000003299760 ) ;
#14811 = AXIS2_PLACEMENT_3D ( 'NONE', #3635, #13529, #480 ) ;
#14812 = CIRCLE ( 'NONE', #16038, 2.649999999999999467 ) ;
#14813 = AXIS2_PLACEMENT_3D ( 'NONE', #8332, #14127, #17100 ) ;
#14814 = DIRECTION ( 'NONE',  ( 0.000000000000000000, 0.000000000000000000, 1.000000000000000000 ) ) ;
#14815 = DIRECTION ( 'NONE',  ( 0.000000000000000000, 0.000000000000000000, 1.000000000000000000 ) ) ;
#14816 = DIRECTION ( 'NONE',  ( 0.000000000000000000, 0.000000000000000000, 1.000000000000000000 ) ) ;
#14817 = EDGE_LOOP ( 'NONE', ( #9558, #16608, #11227, #17926 ) ) ;
#14818 = DIRECTION ( 'NONE',  ( -0.000000000000000000, 1.000000000000000000, -0.000000000000000000 ) ) ;
#14819 = ORIENTED_EDGE ( 'NONE', *, *, #8423, .F. ) ;
#14820 = DIRECTION ( 'NONE',  ( -1.000000000000000000, 0.000000000000000000, 0.000000000000000000 ) ) ;
#14821 = EDGE_LOOP ( 'NONE', ( #908, #14438, #4939, #9044 ) ) ;
#14822 = EDGE_CURVE ( 'NONE', #14354, #4666, #9494, .T. ) ;
#14823 = AXIS2_PLACEMENT_3D ( 'NONE', #3228, #4934, #12356 ) ;
#14824 = EDGE_CURVE ( 'NONE', #808, #15251, #15429, .T. ) ;
#14825 = ADVANCED_FACE ( 'NONE', ( #5502 ), #18259, .F. ) ;
#14826 = CARTESIAN_POINT ( 'NONE',  ( 10.00000000000000000, 46.20417134726178432, -32.31183295104722220 ) ) ;
#14827 = DIRECTION ( 'NONE',  ( -1.000000000000000000, -0.000000000000000000, -0.000000000000000000 ) ) ;
#14828 = CIRCLE ( 'NONE', #7830, 12.00000000001200640 ) ;
#14829 = VERTEX_POINT ( 'NONE', #9780 ) ;
#14830 = ORIENTED_EDGE ( 'NONE', *, *, #9563, .F. ) ;
#14831 = VECTOR ( 'NONE', #9808, 1000.000000000000000 ) ;
#14832 = DIRECTION ( 'NONE',  ( 0.000000000000000000, -1.000000000000000000, 0.000000000000000000 ) ) ;
#14833 = SURFACE_STYLE_USAGE ( .BOTH. , #6068 ) ;
#14834 = EDGE_CURVE ( 'NONE', #9433, #13109, #10920, .T. ) ;
#14835 = ORIENTED_EDGE ( 'NONE', *, *, #2252, .F. ) ;
#14836 = DIRECTION ( 'NONE',  ( 0.000000000000000000, 0.000000000000000000, -1.000000000000000000 ) ) ;
#14837 = AXIS2_PLACEMENT_3D ( 'NONE', #751, #7977, #3790 ) ;
#14838 = AXIS2_PLACEMENT_3D ( 'NONE', #6609, #12511, #5077 ) ;
#14839 = EDGE_CURVE ( 'NONE', #6010, #15825, #14812, .T. ) ;
#14840 = LINE ( 'NONE', #7595, #3500 ) ;
#14841 = VECTOR ( 'NONE', #7729, 999.9999999999998863 ) ;
#14842 = AXIS2_PLACEMENT_3D ( 'NONE', #11266, #8227, #14030 ) ;
#14843 = ORIENTED_EDGE ( 'NONE', *, *, #8192, .F. ) ;
#14844 = ORIENTED_EDGE ( 'NONE', *, *, #6568, .T. ) ;
#14845 = CARTESIAN_POINT ( 'NONE',  ( 10.00000000000000000, -5.120903701083534543E-13, -42.35000000000000142 ) ) ;
#14846 = FACE_OUTER_BOUND ( 'NONE', #10339, .T. ) ;
#14847 = DIRECTION ( 'NONE',  ( 0.000000000000000000, 0.000000000000000000, -1.000000000000000000 ) ) ;
#14848 = VERTEX_POINT ( 'NONE', #8265 ) ;
#14849 = CARTESIAN_POINT ( 'NONE',  ( 4.197393957002303999, 7.772902908466098641E-14, -3.503767560748929810 ) ) ;
#14850 = EDGE_CURVE ( 'NONE', #13753, #8186, #15592, .T. ) ;
#14851 = DIRECTION ( 'NONE',  ( 0.000000000000000000, 0.9510565162951523099, 0.3090169943749515591 ) ) ;
#14852 = CARTESIAN_POINT ( 'NONE',  ( 10.00000000000000000, -33.95787273855213328, -45.00825343885058061 ) ) ;
#14853 = AXIS2_PLACEMENT_3D ( 'NONE', #4416, #7283, #14421 ) ;
#14854 = CARTESIAN_POINT ( 'NONE',  ( 0.000000000000000000, 0.000000000000000000, 0.000000000000000000 ) ) ;
#14855 = EDGE_LOOP ( 'NONE', ( #17252, #5546, #8493 ) ) ;
#14856 = DIRECTION ( 'NONE',  ( 0.000000000000000000, -1.000000000000000000, 0.000000000000000000 ) ) ;
#14857 = CARTESIAN_POINT ( 'NONE',  ( 10.00000000000000000, 5.086963483077590276, -27.72801475327276677 ) ) ;
#14858 = AXIS2_PLACEMENT_3D ( 'NONE', #2795, #8414, #11648 ) ;
#14859 = EDGE_LOOP ( 'NONE', ( #7079, #18556, #595, #11219 ) ) ;
#14860 = CARTESIAN_POINT ( 'NONE',  ( 10.00000000000000000, 55.33199130079785277, 10.11537145609396404 ) ) ;
#14861 = DIRECTION ( 'NONE',  ( -0.000000000000000000, 1.000000000000000000, -0.000000000000000000 ) ) ;
#14862 = MECHANICAL_DESIGN_GEOMETRIC_PRESENTATION_REPRESENTATION (  '', ( #10302 ), #3605 ) ;
#14863 = AXIS2_PLACEMENT_3D ( 'NONE', #1158, #14094, #4013 ) ;
#14864 = EDGE_CURVE ( 'NONE', #560, #1880, #6602, .T. ) ;
#14865 = AXIS2_PLACEMENT_3D ( 'NONE', #6504, #3660, #799 ) ;
#14866 = VERTEX_POINT ( 'NONE', #8352 ) ;
#14867 = VECTOR ( 'NONE', #14304, 1000.000000000000000 ) ;
#14868 = DIRECTION ( 'NONE',  ( 1.000000000000000000, 0.000000000000000000, 0.000000000000000000 ) ) ;
#14869 = LINE ( 'NONE', #7621, #10962 ) ;
#14870 = AXIS2_PLACEMENT_3D ( 'NONE', #9465, #9553, #12140 ) ;
#14871 = COLOUR_RGB ( '',0.8941176470588234615, 0.8941176470588234615, 0.8941176470588234615 ) ;
#14872 = ORIENTED_EDGE ( 'NONE', *, *, #18200, .F. ) ;
#14873 = AXIS2_PLACEMENT_3D ( 'NONE', #1698, #7512, #1886 ) ;
#14874 = DIRECTION ( 'NONE',  ( -1.000000000000000000, -0.000000000000000000, -0.000000000000000000 ) ) ;
#14875 =( REPRESENTATION_RELATIONSHIP ('NONE','NONE', #11014, #8256 ) REPRESENTATION_RELATIONSHIP_WITH_TRANSFORMATION ( #11922 )SHAPE_REPRESENTATION_RELATIONSHIP( ) );
#14876 = DIRECTION ( 'NONE',  ( 0.1305261922200524338, -0.9914448613738102711, 0.000000000000000000 ) ) ;
#14877 = CARTESIAN_POINT ( 'NONE',  ( -79.64793068852898728, -30.00000000000000000, -29.21039329588757383 ) ) ;
#14878 = LINE ( 'NONE', #4586, #8694 ) ;
#14879 = ORIENTED_EDGE ( 'NONE', *, *, #13770, .T. ) ;
#14880 = LINE ( 'NONE', #1914, #1199 ) ;
#14881 = ORIENTED_EDGE ( 'NONE', *, *, #14798, .T. ) ;
#14882 = SHAPE_REPRESENTATION_RELATIONSHIP ( 'NONE' , 'NONE' ,  #16132, #13098 ) ;
#14883 = DIRECTION ( 'NONE',  ( -0.000000000000000000, 1.000000000000000000, -0.000000000000000000 ) ) ;
#14884 = EDGE_LOOP ( 'NONE', ( #6287, #12975 ) ) ;
#14885 = EDGE_CURVE ( 'NONE', #13701, #3414, #11770, .T. ) ;
#14886 = CONTEXT_DEPENDENT_SHAPE_REPRESENTATION ( #14875, #13170 ) ;
#14887 = CIRCLE ( 'NONE', #6671, 2.649999999999985700 ) ;
#14888 = ORIENTED_EDGE ( 'NONE', *, *, #6542, .F. ) ;
#14889 = EDGE_LOOP ( 'NONE', ( #6398, #6447 ) ) ;
#14890 = ORIENTED_EDGE ( 'NONE', *, *, #14083, .F. ) ;
#14891 = DIRECTION ( 'NONE',  ( -1.000000000000000000, -0.000000000000000000, 0.000000000000000000 ) ) ;
#14892 = DIRECTION ( 'NONE',  ( 0.000000000000000000, 0.000000000000000000, -1.000000000000000000 ) ) ;
#14893 = AXIS2_PLACEMENT_3D ( 'NONE', #4852, #12725, #12623 ) ;
#14894 = DIRECTION ( 'NONE',  ( -1.000000000000000000, -0.000000000000000000, -0.000000000000000000 ) ) ;
#14895 = ADVANCED_FACE ( 'NONE', ( #13979 ), #2449, .T. ) ;
#14896 = CARTESIAN_POINT ( 'NONE',  ( 1.411581201560190495E-15, 4.862606272033091592, -3.745885042887436622 ) ) ;
#14897 = AXIS2_PLACEMENT_3D ( 'NONE', #16703, #4887, #15460 ) ;
#14898 = DIRECTION ( 'NONE',  ( 0.000000000000000000, 0.000000000000000000, 1.000000000000000000 ) ) ;
#14899 = CARTESIAN_POINT ( 'NONE',  ( 0.000000000000000000, -1.017308535511979972, -56.37237871411034718 ) ) ;
#14900 = DIRECTION ( 'NONE',  ( 0.000000000000000000, 1.000000000000000000, 3.491481338843133355E-15 ) ) ;
#14901 = PLANE ( 'NONE',  #13046 ) ;
#14902 = VERTEX_POINT ( 'NONE', #5404 ) ;
#14903 = ADVANCED_FACE ( 'NONE', ( #18635 ), #2253, .F. ) ;
#14904 = LINE ( 'NONE', #14993, #3524 ) ;
#14905 = DIRECTION ( 'NONE',  ( 0.1416665029469836024, 0.000000000000000000, 0.9899144417285627995 ) ) ;
#14906 = CYLINDRICAL_SURFACE ( 'NONE', #11794, 56.24900000005625600 ) ;
#14907 = ORIENTED_EDGE ( 'NONE', *, *, #7494, .F. ) ;
#14908 = ORIENTED_EDGE ( 'NONE', *, *, #2432, .F. ) ;
#14909 = CARTESIAN_POINT ( 'NONE',  ( -4.000000000000000000, 2.309401076758498483, -0.4999999999999927280 ) ) ;
#14910 = CARTESIAN_POINT ( 'NONE',  ( -79.64793068852927149, -25.00000000000000000, 31.86039329588764701 ) ) ;
#14911 = CARTESIAN_POINT ( 'NONE',  ( 0.000000000000000000, 1.305124410222461284, 0.000000000000000000 ) ) ;
#14912 = VERTEX_POINT ( 'NONE', #12636 ) ;
#14913 = CIRCLE ( 'NONE', #9119, 2.649999999999985700 ) ;
#14914 = AXIS2_PLACEMENT_3D ( 'NONE', #2519, #9948, #14048 ) ;
#14915 = FACE_OUTER_BOUND ( 'NONE', #9507, .T. ) ;
#14916 = LINE ( 'NONE', #13397, #17487 ) ;
#14917 = FACE_OUTER_BOUND ( 'NONE', #15952, .T. ) ;
#14918 = EDGE_LOOP ( 'NONE', ( #8236, #8366, #14644, #10807 ) ) ;
#14919 = CARTESIAN_POINT ( 'NONE',  ( 10.00000000000000000, -41.62350880771888484, -47.29147401531998440 ) ) ;
#14920 = ORIENTED_EDGE ( 'NONE', *, *, #10755, .F. ) ;
#14921 = CARTESIAN_POINT ( 'NONE',  ( -0.1481481481481481122, -4.797713218419819903, 0.000000000000000000 ) ) ;
#14922 = ORIENTED_EDGE ( 'NONE', *, *, #5588, .T. ) ;
#14923 = CIRCLE ( 'NONE', #13406, 24.00000000002399858 ) ;
#14924 = CYLINDRICAL_SURFACE ( 'NONE', #3021, 2.649999999999992806 ) ;
#14925 = DIRECTION ( 'NONE',  ( 0.000000000000000000, 0.000000000000000000, 1.000000000000000000 ) ) ;
#14926 = ORIENTED_EDGE ( 'NONE', *, *, #4357, .F. ) ;
#14927 = ORIENTED_EDGE ( 'NONE', *, *, #5588, .F. ) ;
#14928 = FACE_OUTER_BOUND ( 'NONE', #15513, .T. ) ;
#14929 = PRESENTATION_STYLE_ASSIGNMENT (( #15217 ) ) ;
#14930 = ORIENTED_EDGE ( 'NONE', *, *, #1801, .F. ) ;
#14931 = DIRECTION ( 'NONE',  ( -1.000000000000000000, 0.000000000000000000, -0.000000000000000000 ) ) ;
#14932 = ADVANCED_FACE ( 'NONE', ( #6647 ), #11105, .T. ) ;
#14933 = EDGE_CURVE ( 'NONE', #4445, #380, #3563, .T. ) ;
#14934 = AXIS2_PLACEMENT_3D ( 'NONE', #13160, #10199, #16012 ) ;
#14935 = DIRECTION ( 'NONE',  ( 0.000000000000000000, 0.000000000000000000, -1.000000000000000000 ) ) ;
#14936 = EDGE_CURVE ( 'NONE', #8859, #2515, #4435, .T. ) ;
#14937 = ORIENTED_EDGE ( 'NONE', *, *, #729, .F. ) ;
#14938 = EDGE_CURVE ( 'NONE', #10240, #9460, #13020, .T. ) ;
#14939 = EDGE_LOOP ( 'NONE', ( #17021, #6256, #8198, #13667 ) ) ;
#14940 = DIRECTION ( 'NONE',  ( 0.000000000000000000, 0.000000000000000000, -1.000000000000000000 ) ) ;
#14941 = DIRECTION ( 'NONE',  ( -0.000000000000000000, 1.000000000000000000, -0.000000000000000000 ) ) ;
#14942 = FACE_OUTER_BOUND ( 'NONE', #13833, .T. ) ;
#14943 = ORIENTED_EDGE ( 'NONE', *, *, #15339, .T. ) ;
#14944 = DIRECTION ( 'NONE',  ( 0.000000000000000000, 0.000000000000000000, 1.000000000000000000 ) ) ;
#14945 = CARTESIAN_POINT ( 'NONE',  ( 2.855764796983346177, -2.970025579236428737, -0.09382832055446485575 ) ) ;
#14946 = DIRECTION ( 'NONE',  ( 0.000000000000000000, -1.000000000000000000, 1.287488025362403787E-15 ) ) ;
#14947 = FACE_OUTER_BOUND ( 'NONE', #18647, .T. ) ;
#14948 = ORIENTED_EDGE ( 'NONE', *, *, #11950, .F. ) ;
#14949 = CARTESIAN_POINT ( 'NONE',  ( 10.00000000000000000, -27.94286728106390072, -3.730438010304629515 ) ) ;
#14950 = CIRCLE ( 'NONE', #3392, 24.00000000002399858 ) ;
#14951 = DIRECTION ( 'NONE',  ( -1.000000000000000000, -0.000000000000000000, -0.000000000000000000 ) ) ;
#14953 = EDGE_CURVE ( 'NONE', #7648, #4230, #18791, .T. ) ;
#14952 = EDGE_LOOP ( 'NONE', ( #12207, #12968, #6259, #3456 ) ) ;
#14954 = CARTESIAN_POINT ( 'NONE',  ( 0.000000000000000000, 0.000000000000000000, 0.000000000000000000 ) ) ;
#14955 = DIRECTION ( 'NONE',  ( -0.000000000000000000, 1.000000000000000000, -0.000000000000000000 ) ) ;
#14956 = AXIS2_PLACEMENT_3D ( 'NONE', #32, #10205, #1183 ) ;
#14957 = B_SPLINE_CURVE_WITH_KNOTS ( 'NONE', 3,
 ( #13248, #6004, #13355, #302, #3440, #387 ),
 .UNSPECIFIED., .F., .F.,
 ( 4, 2, 4 ),
 ( 0.000000000000000000, 0.0002095117440864791795, 0.0004190234881729583589 ),
 .UNSPECIFIED. ) ;
#14958 = EDGE_CURVE ( 'NONE', #8129, #10560, #10247, .T. ) ;
#14959 = EDGE_CURVE ( 'NONE', #6509, #11571, #4265, .T. ) ;
#14960 = ORIENTED_EDGE ( 'NONE', *, *, #7423, .F. ) ;
#14961 = SURFACE_STYLE_USAGE ( .BOTH. , #9143 ) ;
#14962 = ORIENTED_EDGE ( 'NONE', *, *, #1661, .F. ) ;
#14963 = DIRECTION ( 'NONE',  ( -0.000000000000000000, 1.000000000000000000, -0.000000000000000000 ) ) ;
#14964 = ADVANCED_FACE ( 'NONE', ( #2824 ), #11594, .F. ) ;
#14965 = DIRECTION ( 'NONE',  ( -0.000000000000000000, -1.000000000000000000, -0.000000000000000000 ) ) ;
#14966 = AXIS2_PLACEMENT_3D ( 'NONE', #1056, #4014, #9902 ) ;
#14967 = CYLINDRICAL_SURFACE ( 'NONE', #17310, 33.00000000003299760 ) ;
#14968 = FACE_OUTER_BOUND ( 'NONE', #11435, .T. ) ;
#14969 = CARTESIAN_POINT ( 'NONE',  ( 0.000000000000000000, 24.97244012287502102, 57.83923611457328207 ) ) ;
#14970 = ORIENTED_EDGE ( 'NONE', *, *, #9641, .T. ) ;
#14971 = FACE_OUTER_BOUND ( 'NONE', #13747, .T. ) ;
#14972 = ORIENTED_EDGE ( 'NONE', *, *, #2262, .F. ) ;
#14973 = AXIS2_PLACEMENT_3D ( 'NONE', #15366, #10982, #3756 ) ;
#14974 = LINE ( 'NONE', #4776, #14247 ) ;
#14975 = EDGE_LOOP ( 'NONE', ( #7509, #2450 ) ) ;
#14976 = ITEM_DEFINED_TRANSFORMATION ( 'NONE', 'NONE', #10189,  #8017 ) ;
#14977 = ORIENTED_EDGE ( 'NONE', *, *, #11018, .F. ) ;
#14978 = ORIENTED_EDGE ( 'NONE', *, *, #9689, .F. ) ;
#14979 = APPLICATION_CONTEXT ( 'automotive_design' ) ;
#14980 = VERTEX_POINT ( 'NONE', #4351 ) ;
#14981 = CARTESIAN_POINT ( 'NONE',  ( 0.000000000000000000, -30.00000000000000000, 25.00000000000000000 ) ) ;
#14982 = CYLINDRICAL_SURFACE ( 'NONE', #6715, 12.00000000001200462 ) ;
#14983 = CARTESIAN_POINT ( 'NONE',  ( 3.367778697655221307E-15, -17.25000000000000355, -27.50000000000000000 ) ) ;
#14984 = EDGE_CURVE ( 'NONE', #10779, #15019, #10151, .T. ) ;
#14985 = CARTESIAN_POINT ( 'NONE',  ( -87.76214430591549842, 2.081668171172168513E-14, 4.471241649927989670 ) ) ;
#14986 = CYLINDRICAL_SURFACE ( 'NONE', #548, 2.500000000000000444 ) ;
#14987 = DIRECTION ( 'NONE',  ( -1.000000000000000000, 0.000000000000000000, 0.000000000000000000 ) ) ;
#14988 = CARTESIAN_POINT ( 'NONE',  ( -4.000000000000000000, 2.309401076758498483, -3.433295621305379353 ) ) ;
#14989 = ORIENTED_EDGE ( 'NONE', *, *, #5174, .T. ) ;
#14990 = CARTESIAN_POINT ( 'NONE',  ( 0.000000000000000000, -30.00000000000000000, 0.000000000000000000 ) ) ;
#14991 = ORIENTED_EDGE ( 'NONE', *, *, #5154, .F. ) ;
#14992 = AXIS2_PLACEMENT_3D ( 'NONE', #18562, #8277, #6657 ) ;
#14993 = CARTESIAN_POINT ( 'NONE',  ( 10.00000000000000000, 53.89344778774812994, 16.10733642026502466 ) ) ;
#14994 = CARTESIAN_POINT ( 'NONE',  ( 0.000000000000000000, 23.24033432160437584, 58.55669782892469755 ) ) ;
#14995 = VECTOR ( 'NONE', #10688, 1000.000000000000000 ) ;
#14996 = DIRECTION ( 'NONE',  ( -1.000000000000000000, -0.000000000000000000, -0.000000000000000000 ) ) ;
#14997 = VERTEX_POINT ( 'NONE', #13297 ) ;
#14998 = EDGE_LOOP ( 'NONE', ( #3290, #7955, #3770, #8615 ) ) ;
#14999 = CIRCLE ( 'NONE', #6777, 55.00000000000000000 ) ;
#15000 = CARTESIAN_POINT ( 'NONE',  ( -2.345747346278108214, 3.264484291692489215, -0.01223254789873409049 ) ) ;
#15001 = DIRECTION ( 'NONE',  ( 0.9995004958639134296, 0.000000000000000000, 0.03160314490350069061 ) ) ;
#15002 = CARTESIAN_POINT ( 'NONE',  ( -1.128893538851230005, 13.24999999999999467, 23.47286943213250154 ) ) ;
#15003 = ORIENTED_EDGE ( 'NONE', *, *, #1490, .F. ) ;
#15004 = ADVANCED_FACE ( 'NONE', ( #1581 ), #17318, .T. ) ;
#15005 = PRODUCT_DEFINITION_SHAPE ( 'NONE', 'NONE',  #18817 ) ;
#15006 = ADVANCED_FACE ( 'NONE', ( #5949 ), #8626, .T. ) ;
#15007 = VECTOR ( 'NONE', #8552, 1000.000000000000000 ) ;
#15008 = DIRECTION ( 'NONE',  ( -1.000000000000000000, 0.000000000000000000, 0.000000000000000000 ) ) ;
#15009 = FACE_BOUND ( 'NONE', #15476, .T. ) ;
#15010 = VECTOR ( 'NONE', #16478, 1000.000000000000000 ) ;
#15011 = FACE_OUTER_BOUND ( 'NONE', #4960, .T. ) ;
#15012 = ORIENTED_EDGE ( 'NONE', *, *, #16270, .F. ) ;
#15013 = FACE_OUTER_BOUND ( 'NONE', #12597, .T. ) ;
#15014 = ORIENTED_EDGE ( 'NONE', *, *, #8041, .F. ) ;
#15015 = LINE ( 'NONE', #2060, #10589 ) ;
#15016 = ORIENTED_EDGE ( 'NONE', *, *, #14121, .T. ) ;
#15017 = DIRECTION ( 'NONE',  ( 0.000000000000000000, 0.000000000000000000, 1.000000000000000000 ) ) ;
#15018 = CYLINDRICAL_SURFACE ( 'NONE', #9826, 63.00000000006298961 ) ;
#15019 = VERTEX_POINT ( 'NONE', #4536 ) ;
#15020 = ORIENTED_EDGE ( 'NONE', *, *, #14074, .T. ) ;
#15021 = CARTESIAN_POINT ( 'NONE',  ( -90.00000000009001155, -49.14213562373095812, -1.301042606982603940E-15 ) ) ;
#15022 = SURFACE_STYLE_FILL_AREA ( #444 ) ;
#15023 = VECTOR ( 'NONE', #14905, 1000.000000000000227 ) ;
#15024 = VERTEX_POINT ( 'NONE', #16156 ) ;
#15025 = DIRECTION ( 'NONE',  ( 0.000000000000000000, 0.000000000000000000, 1.000000000000000000 ) ) ;
#15026 = DIRECTION ( 'NONE',  ( -1.000000000000000000, -0.000000000000000000, 0.000000000000000000 ) ) ;
#15027 = EDGE_LOOP ( 'NONE', ( #5054, #14927, #9894, #1753 ) ) ;
#15028 =( GEOMETRIC_REPRESENTATION_CONTEXT ( 3 ) GLOBAL_UNCERTAINTY_ASSIGNED_CONTEXT ( ( #13766 ) ) GLOBAL_UNIT_ASSIGNED_CONTEXT ( ( #486, #13258, #6396 ) ) REPRESENTATION_CONTEXT ( 'NONE', 'WORKASPACE' ) );
#15029 = ORIENTED_EDGE ( 'NONE', *, *, #9274, .F. ) ;
#15030 = CARTESIAN_POINT ( 'NONE',  ( 10.00000000000000000, -32.31183295104805353, 46.20417134726119457 ) ) ;
#15031 = CARTESIAN_POINT ( 'NONE',  ( 0.000000000000000000, 0.000000000000000000, 0.000000000000000000 ) ) ;
#15032 = CARTESIAN_POINT ( 'NONE',  ( 27.29487558977753991, 1.305124410222461284, -2.000000000000000000 ) ) ;
#15033 = ORIENTED_EDGE ( 'NONE', *, *, #4668, .F. ) ;
#15034 = CARTESIAN_POINT ( 'NONE',  ( 0.000000000000000000, 0.000000000000000000, 0.000000000000000000 ) ) ;
#15035 = CARTESIAN_POINT ( 'NONE',  ( 0.000000000000000000, 4.381479206522993941, 32.70783759231088084 ) ) ;
#15036 = CYLINDRICAL_SURFACE ( 'NONE', #14065, 63.00000000006298961 ) ;
#15037 = FACE_OUTER_BOUND ( 'NONE', #15602, .T. ) ;
#15038 = ORIENTED_EDGE ( 'NONE', *, *, #9720, .T. ) ;
#15039 = EDGE_CURVE ( 'NONE', #4267, #726, #4786, .T. ) ;
#15040 = CARTESIAN_POINT ( 'NONE',  ( 0.2500000000000002220, 0.000000000000000000, 4.250000000000000000 ) ) ;
#15041 = EDGE_CURVE ( 'NONE', #8001, #5512, #5997, .T. ) ;
#15042 = ORIENTED_EDGE ( 'NONE', *, *, #2891, .F. ) ;
#15043 = DIRECTION ( 'NONE',  ( 0.000000000000000000, 0.3090169943749481174, -0.9510565162951533091 ) ) ;
#15044 = CARTESIAN_POINT ( 'NONE',  ( 4.999999999999999112, -62.72529079327802748, -5.876895005583096854 ) ) ;
#15045 = PRODUCT_RELATED_PRODUCT_CATEGORY ( 'part', '', ( #4043 ) ) ;
#15046 = VECTOR ( 'NONE', #3416, 1000.000000000000000 ) ;
#15047 = EDGE_CURVE ( 'NONE', #16590, #18403, #18165, .T. ) ;
#15048 = ORIENTED_EDGE ( 'NONE', *, *, #13816, .F. ) ;
#15049 = DIRECTION ( 'NONE',  ( 0.000000000000000000, 0.000000000000000000, -1.000000000000000000 ) ) ;
#15050 = EDGE_CURVE ( 'NONE', #8889, #5171, #14828, .T. ) ;
#15051 = ORIENTED_EDGE ( 'NONE', *, *, #12092, .T. ) ;
#15052 = LINE ( 'NONE', #12192, #10610 ) ;
#15053 = CARTESIAN_POINT ( 'NONE',  ( 32.50000000000000000, -30.00000000000000000, 2.650000000000367617 ) ) ;
#15054 = AXIS2_PLACEMENT_3D ( 'NONE', #7571, #13390, #7743 ) ;
#15055 = FACE_OUTER_BOUND ( 'NONE', #12159, .T. ) ;
#15056 = CARTESIAN_POINT ( 'NONE',  ( 5.000000000000000000, -58.55669782892479702, 23.24033432160415913 ) ) ;
#15057 = CIRCLE ( 'NONE', #12625, 12.00000000001200462 ) ;
#15058 = CARTESIAN_POINT ( 'NONE',  ( -117.1020693116508085, -30.00000000000000000, 22.34080595179777262 ) ) ;
#15059 = EDGE_LOOP ( 'NONE', ( #14682, #14546, #15255, #5189 ) ) ;
#15060 = CARTESIAN_POINT ( 'NONE',  ( -26.29305231718568336, -26.50000000000000000, -16.45302069950552237 ) ) ;
#15061 = EDGE_CURVE ( 'NONE', #2107, #3517, #15959, .T. ) ;
#15062 = EDGE_CURVE ( 'NONE', #3659, #13804, #16647, .T. ) ;
#15063 = CARTESIAN_POINT ( 'NONE',  ( 0.000000000000000000, -6.681932690256794594, -25.38428207620328791 ) ) ;
#15064 = VERTEX_POINT ( 'NONE', #14431 ) ;
#15065 = EDGE_CURVE ( 'NONE', #13152, #14782, #7150, .T. ) ;
#15066 = ORIENTED_EDGE ( 'NONE', *, *, #7377, .F. ) ;
#15067 = EDGE_CURVE ( 'NONE', #6939, #14764, #5710, .T. ) ;
#15068 = AXIS2_PLACEMENT_3D ( 'NONE', #4048, #11175, #18517 ) ;
#15069 = EDGE_LOOP ( 'NONE', ( #14521, #16010, #8842, #12519 ) ) ;
#15070 = AXIS2_PLACEMENT_3D ( 'NONE', #6142, #1857, #7660 ) ;
#15071 = VECTOR ( 'NONE', #5557, 1000.000000000000000 ) ;
#15072 = ORIENTED_EDGE ( 'NONE', *, *, #9627, .F. ) ;
#15073 = ADVANCED_FACE ( 'NONE', ( #15011 ), #13583, .F. ) ;
#15074 = CARTESIAN_POINT ( 'NONE',  ( -90.00000000009001155, -88.00000000000000000, -1.301042606982603940E-15 ) ) ;
#15075 = DIRECTION ( 'NONE',  ( 0.000000000000000000, 0.000000000000000000, 1.000000000000000000 ) ) ;
#15076 = DIRECTION ( 'NONE',  ( 0.000000000000000000, 0.000000000000000000, 1.000000000000000000 ) ) ;
#15077 = DIRECTION ( 'NONE',  ( 0.1305261922200516844, -0.9914448613738103822, 0.000000000000000000 ) ) ;
#15078 = DIRECTION ( 'NONE',  ( 1.000000000000000000, -0.000000000000000000, 0.000000000000000000 ) ) ;
#15079 = DIRECTION ( 'NONE',  ( 0.000000000000000000, 0.000000000000000000, 1.000000000000000000 ) ) ;
#15080 = DIRECTION ( 'NONE',  ( -0.000000000000000000, 1.000000000000000000, -0.000000000000000000 ) ) ;
#15081 = CIRCLE ( 'NONE', #11739, 24.00000000002399858 ) ;
#15082 = FACE_OUTER_BOUND ( 'NONE', #9549, .T. ) ;
#15083 = ORIENTED_EDGE ( 'NONE', *, *, #6140, .F. ) ;
#15084 = CARTESIAN_POINT ( 'NONE',  ( 5.000000000000000000, 57.83923611457320391, 24.97244012287522352 ) ) ;
#15085 = MECHANICAL_DESIGN_GEOMETRIC_PRESENTATION_REPRESENTATION (  '', ( #3839 ), #14478 ) ;
#15086 = ORIENTED_EDGE ( 'NONE', *, *, #12907, .F. ) ;
#15087 = ORIENTED_EDGE ( 'NONE', *, *, #174, .T. ) ;
#15088 = CARTESIAN_POINT ( 'NONE',  ( -79.64793068852927149, -30.00000000000000000, 34.51039329588763849 ) ) ;
#15089 = DIRECTION ( 'NONE',  ( 0.000000000000000000, 0.1564344650402312298, -0.9876883405951376593 ) ) ;
#15090 = DIRECTION ( 'NONE',  ( -0.000000000000000000, 1.000000000000000000, -0.000000000000000000 ) ) ;
#15091 = VERTEX_POINT ( 'NONE', #4906 ) ;
#15092 = VECTOR ( 'NONE', #17738, 1000.000000000000000 ) ;
#15093 = VERTEX_POINT ( 'NONE', #6054 ) ;
#15094 = VECTOR ( 'NONE', #883, 1000.000000000000000 ) ;
#15095 = DIRECTION ( 'NONE',  ( -1.000000000000000000, 0.000000000000000000, 0.000000000000000000 ) ) ;
#15096 = DIRECTION ( 'NONE',  ( 6.123233995736766036E-17, -1.000000000000000000, 0.000000000000000000 ) ) ;
#15097 = CARTESIAN_POINT ( 'NONE',  ( 10.00000000000000000, 16.45250512421856470, 53.92768374110897156 ) ) ;
#15098 = ORIENTED_EDGE ( 'NONE', *, *, #10423, .F. ) ;
#15099 = ADVANCED_FACE ( 'NONE', ( #16343 ), #6429, .T. ) ;
#15100 = CIRCLE ( 'NONE', #2010, 27.29487558977753991 ) ;
#15101 = AXIS2_PLACEMENT_3D ( 'NONE', #14857, #7696, #13519 ) ;
#15102 = CIRCLE ( 'NONE', #2312, 24.00000000002400213 ) ;
#15103 = FACE_OUTER_BOUND ( 'NONE', #14147, .T. ) ;
#15104 = DIRECTION ( 'NONE',  ( 0.000000000000000000, 1.000000000000000000, 0.000000000000000000 ) ) ;
#15105 = VECTOR ( 'NONE', #2496, 1000.000000000000000 ) ;
#15106 = AXIS2_PLACEMENT_3D ( 'NONE', #14826, #4632, #16447 ) ;
#15107 = FACE_OUTER_BOUND ( 'NONE', #9881, .T. ) ;
#15108 = VERTEX_POINT ( 'NONE', #7752 ) ;
#15109 = DIRECTION ( 'NONE',  ( 0.000000000000000000, 0.000000000000000000, 1.000000000000000000 ) ) ;
#15110 = EDGE_LOOP ( 'NONE', ( #9065, #212, #9343, #6639 ) ) ;
#15111 = UNCERTAINTY_MEASURE_WITH_UNIT (LENGTH_MEASURE( 1.000000000000000082E-05 ), #16276, 'distance_accuracy_value', 'NONE');
#15112 = FACE_BOUND ( 'NONE', #5366, .T. ) ;
#15113 = ORIENTED_EDGE ( 'NONE', *, *, #13439, .T. ) ;
#15114 = DIRECTION ( 'NONE',  ( -1.000000000000000000, 0.000000000000000000, -0.000000000000000000 ) ) ;
#15115 = CARTESIAN_POINT ( 'NONE',  ( 0.02448733951239481094, 4.877042772274728044, -3.751161874094022242 ) ) ;
#15116 = ORIENTED_EDGE ( 'NONE', *, *, #7257, .T. ) ;
#15117 = ORIENTED_EDGE ( 'NONE', *, *, #1391, .T. ) ;
#15118 = DIRECTION ( 'NONE',  ( -0.000000000000000000, 1.000000000000000000, -0.000000000000000000 ) ) ;
#15119 = AXIS2_PLACEMENT_3D ( 'NONE', #9721, #1157, #4099 ) ;
#15120 = ORIENTED_EDGE ( 'NONE', *, *, #5338, .T. ) ;
#15121 = FACE_OUTER_BOUND ( 'NONE', #6209, .T. ) ;
#15122 = CIRCLE ( 'NONE', #12070, 24.00000000002400213 ) ;
#15123 = AXIS2_PLACEMENT_3D ( 'NONE', #3634, #9428, #15246 ) ;
#15124 = EDGE_CURVE ( 'NONE', #3205, #980, #15447, .T. ) ;
#15125 = DIRECTION ( 'NONE',  ( -0.000000000000000000, 1.000000000000000000, -0.000000000000000000 ) ) ;
#15126 = CIRCLE ( 'NONE', #9330, 24.00000000002399858 ) ;
#15127 = ORIENTED_EDGE ( 'NONE', *, *, #3460, .F. ) ;
#15128 = CIRCLE ( 'NONE', #3580, 24.00000000002399858 ) ;
#15129 = AXIS2_PLACEMENT_3D ( 'NONE', #3200, #10523, #4818 ) ;
#15130 = EDGE_LOOP ( 'NONE', ( #18467, #9058 ) ) ;
#15131 = DIRECTION ( 'NONE',  ( 0.000000000000000000, -6.938893903900288768E-15, 1.000000000000000000 ) ) ;
#15132 = AXIS2_PLACEMENT_3D ( 'NONE', #17565, #11753, #12745 ) ;
#15133 = CARTESIAN_POINT ( 'NONE',  ( 10.00000000000000000, -19.44239304137390434, 20.41355805489607889 ) ) ;
#15134 = DIRECTION ( 'NONE',  ( -1.000000000000000000, -0.000000000000000000, -0.000000000000000000 ) ) ;
#15135 = ADVANCED_FACE ( 'NONE', ( #16528 ), #13680, .T. ) ;
#15136 = ORIENTED_EDGE ( 'NONE', *, *, #7823, .F. ) ;
#15137 = DIRECTION ( 'NONE',  ( 0.000000000000000000, 0.000000000000000000, -1.000000000000000000 ) ) ;
#15138 = FACE_OUTER_BOUND ( 'NONE', #14939, .T. ) ;
#15139 = CARTESIAN_POINT ( 'NONE',  ( 13.90576474687299680, 10.00000000000000000, 42.79754323328179311 ) ) ;
#15140 = CARTESIAN_POINT ( 'NONE',  ( 0.000000000000000000, 0.000000000000000000, 0.000000000000000000 ) ) ;
#15141 = ORIENTED_EDGE ( 'NONE', *, *, #14665, .F. ) ;
#15142 = DIRECTION ( 'NONE',  ( 0.000000000000000000, 0.000000000000000000, 1.000000000000000000 ) ) ;
#15143 = EDGE_CURVE ( 'NONE', #17590, #16428, #16245, .T. ) ;
#15144 = ORIENTED_EDGE ( 'NONE', *, *, #15830, .F. ) ;
#15145 = CARTESIAN_POINT ( 'NONE',  ( 0.000000000000000000, 2.357898499370432166, -2.385244779468109755E-15 ) ) ;
#15146 = LINE ( 'NONE', #10661, #15010 ) ;
#15147 = AXIS2_PLACEMENT_3D ( 'NONE', #14634, #4439, #13027 ) ;
#15148 = CIRCLE ( 'NONE', #16365, 33.00000000003299760 ) ;
#15149 = VECTOR ( 'NONE', #5844, 1000.000000000000000 ) ;
#15150 = AXIS2_PLACEMENT_3D ( 'NONE', #16487, #12195, #3353 ) ;
#15151 = EDGE_LOOP ( 'NONE', ( #6604, #2921, #4253, #3577, #17748 ) ) ;
#15152 = VECTOR ( 'NONE', #4252, 1000.000000000000000 ) ;
#15153 = VERTEX_POINT ( 'NONE', #627 ) ;
#15154 = LINE ( 'NONE', #16771, #12132 ) ;
#15155 = CARTESIAN_POINT ( 'NONE',  ( -0.5000000000000000000, -30.39588787977742257, 0.000000000000000000 ) ) ;
#15156 = DIRECTION ( 'NONE',  ( 0.000000000000000000, 0.000000000000000000, 1.000000000000000000 ) ) ;
#15157 = CIRCLE ( 'NONE', #9067, 56.24900000005625600 ) ;
#15158 = CYLINDRICAL_SURFACE ( 'NONE', #9376, 23.50000000000001066 ) ;
#15159 = CIRCLE ( 'NONE', #11207, 33.00000000003299760 ) ;
#15160 = DIRECTION ( 'NONE',  ( -0.000000000000000000, 1.000000000000000000, 1.224646799147353207E-16 ) ) ;
#15161 = ORIENTED_EDGE ( 'NONE', *, *, #15519, .T. ) ;
#15162 = VECTOR ( 'NONE', #18762, 1000.000000000000000 ) ;
#15163 = CARTESIAN_POINT ( 'NONE',  ( 20.55500000000001748, 3.061616997868384127E-16, -2.500000000000000888 ) ) ;
#15164 = PRODUCT_DEFINITION_SHAPE ( 'NONE', 'NONE',  #18842 ) ;
#15165 =( NAMED_UNIT ( * ) SI_UNIT ( $, .STERADIAN. ) SOLID_ANGLE_UNIT ( ) );
#15166 = CARTESIAN_POINT ( 'NONE',  ( 4.999999999999999112, -15.61693798565540270, 61.03368945066429774 ) ) ;
#15167 = VERTEX_POINT ( 'NONE', #10620 ) ;
#15168 = VERTEX_POINT ( 'NONE', #6342 ) ;
#15169 = AXIS2_PLACEMENT_3D ( 'NONE', #52, #11662, #12909 ) ;
#15170 = AXIS2_PLACEMENT_3D ( 'NONE', #7899, #9419, #5222 ) ;
#15171 = EDGE_LOOP ( 'NONE', ( #17244, #18058, #2133, #13203 ) ) ;
#15172 = AXIS2_PLACEMENT_3D ( 'NONE', #6269, #659, #11806 ) ;
#15173 = EDGE_CURVE ( 'NONE', #6648, #14229, #18045, .T. ) ;
#15174 = EDGE_CURVE ( 'NONE', #380, #8389, #4711, .T. ) ;
#15175 = ORIENTED_EDGE ( 'NONE', *, *, #18805, .F. ) ;
#15176 = CARTESIAN_POINT ( 'NONE',  ( -36.40576474687247099, 10.00000000000000000, 23.80033635316149443 ) ) ;
#15177 = ADVANCED_FACE ( 'NONE', ( #14917 ), #3483, .F. ) ;
#15178 = SURFACE_STYLE_USAGE ( .BOTH. , #501 ) ;
#15179 = FACE_OUTER_BOUND ( 'NONE', #1397, .T. ) ;
#15180 = DIRECTION ( 'NONE',  ( 0.000000000000000000, 0.9510565162951545304, -0.3090169943749446202 ) ) ;
#15181 =( NAMED_UNIT ( * ) PLANE_ANGLE_UNIT ( ) SI_UNIT ( $, .RADIAN. ) );
#15182 = ADVANCED_FACE ( 'NONE', ( #9277 ), #7662, .F. ) ;
#15183 = DIRECTION ( 'NONE',  ( 0.000000000000000000, 0.000000000000000000, 1.000000000000000000 ) ) ;
#15184 = AXIS2_PLACEMENT_3D ( 'NONE', #4318, #11457, #5832 ) ;
#15185 = CARTESIAN_POINT ( 'NONE',  ( -79.64793068852927149, -30.00000000000000000, 31.86039329588764701 ) ) ;
#15186 = LINE ( 'NONE', #16506, #12319 ) ;
#15187 = ORIENTED_EDGE ( 'NONE', *, *, #10039, .T. ) ;
#15188 = CARTESIAN_POINT ( 'NONE',  ( 0.000000000000000000, 0.5192545390863916310, -1.000000000000000000 ) ) ;
#15189 = ORIENTED_EDGE ( 'NONE', *, *, #18202, .T. ) ;
#15190 = AXIS2_PLACEMENT_3D ( 'NONE', #11231, #11122, #8558 ) ;
#15191 = EDGE_CURVE ( 'NONE', #5117, #7622, #13923, .T. ) ;
#15192 = DIRECTION ( 'NONE',  ( 0.000000000000000000, 0.000000000000000000, 1.000000000000000000 ) ) ;
#15193 = DIRECTION ( 'NONE',  ( 0.000000000000000000, 0.000000000000000000, 1.000000000000000000 ) ) ;
#15194 = ORIENTED_EDGE ( 'NONE', *, *, #8212, .F. ) ;
#15195 = ORIENTED_EDGE ( 'NONE', *, *, #5499, .F. ) ;
#15196 = CARTESIAN_POINT ( 'NONE',  ( -4.000000000000000000, 2.309401076758498483, -5.000000000000000000 ) ) ;
#15197 = DIRECTION ( 'NONE',  ( 0.000000000000000000, 0.000000000000000000, 1.000000000000000000 ) ) ;
#15198 = CARTESIAN_POINT ( 'NONE',  ( 50.00005079999999680, 6.799999999999999822, 1.500000000000000000 ) ) ;
#15199 = ORIENTED_EDGE ( 'NONE', *, *, #6714, .T. ) ;
#15200 = ADVANCED_FACE ( 'NONE', ( #15107 ), #16621, .T. ) ;
#15201 = CIRCLE ( 'NONE', #296, 1.250000000000001110 ) ;
#15202 = DIRECTION ( 'NONE',  ( 0.000000000000000000, 0.000000000000000000, -1.000000000000000000 ) ) ;
#15203 = DIRECTION ( 'NONE',  ( -0.5000000000000051070, 1.060575238724903217E-16, -0.8660254037844355990 ) ) ;
#15204 = CARTESIAN_POINT ( 'NONE',  ( -10.00000000000000000, 0.000000000000000000, 0.000000000000000000 ) ) ;
#15205 = ORIENTED_EDGE ( 'NONE', *, *, #396, .T. ) ;
#15206 = CARTESIAN_POINT ( 'NONE',  ( 10.00000000000000000, -9.514709542737069370, 24.46385708179980512 ) ) ;
#15207 = VERTEX_POINT ( 'NONE', #7578 ) ;
#15208 = DIRECTION ( 'NONE',  ( 0.000000000000000000, -1.000000000000000000, 0.000000000000000000 ) ) ;
#15209 = VERTEX_POINT ( 'NONE', #13398 ) ;
#15210 = ADVANCED_FACE ( 'NONE', ( #345 ), #6144, .T. ) ;
#15211 = DIRECTION ( 'NONE',  ( 0.000000000000000000, 1.000000000000000000, 0.000000000000000000 ) ) ;
#15212 = CYLINDRICAL_SURFACE ( 'NONE', #1610, 24.00000000002400213 ) ;
#15213 = VERTEX_POINT ( 'NONE', #6236 ) ;
#15214 = EDGE_LOOP ( 'NONE', ( #9486, #3077 ) ) ;
#15215 = CARTESIAN_POINT ( 'NONE',  ( 0.000000000000000000, -17.25000000000000355, 0.000000000000000000 ) ) ;
#15216 = VECTOR ( 'NONE', #18218, 1000.000000000000000 ) ;
#15217 = SURFACE_STYLE_USAGE ( .BOTH. , #13694 ) ;
#15218 = EDGE_LOOP ( 'NONE', ( #10029, #13264, #2248, #18694 ) ) ;
#15219 = CARTESIAN_POINT ( 'NONE',  ( 10.00000000000000000, -15.68049343255974826, -29.03656532225580733 ) ) ;
#15220 = CARTESIAN_POINT ( 'NONE',  ( -90.00000000009001155, -49.14213562373095812, 5.000000000000003553 ) ) ;
#15221 = AXIS2_PLACEMENT_3D ( 'NONE', #13182, #17834, #14696 ) ;
#15222 = CARTESIAN_POINT ( 'NONE',  ( -6.080745460913608902, 0.5192545390863924082, -1.000000000000000000 ) ) ;
#15223 = ORIENTED_EDGE ( 'NONE', *, *, #18677, .F. ) ;
#15224 = CIRCLE ( 'NONE', #7618, 6.080745460913608902 ) ;
#15225 = VERTEX_POINT ( 'NONE', #12045 ) ;
#15226 = CARTESIAN_POINT ( 'NONE',  ( 10.00000000000000000, -5.086963483077008519, -27.72801475327286980 ) ) ;
#15227 = CARTESIAN_POINT ( 'NONE',  ( -97.50000000009001155, -13.00000000000001599, -1.496198998029995922E-15 ) ) ;
#15228 = ORIENTED_EDGE ( 'NONE', *, *, #12328, .T. ) ;
#15229 = LINE ( 'NONE', #753, #1148 ) ;
#15230 = EDGE_CURVE ( 'NONE', #3488, #17821, #16438, .T. ) ;
#15231 = LINE ( 'NONE', #18459, #268 ) ;
#15232 = DIRECTION ( 'NONE',  ( 0.000000000000000000, -1.000000000000000000, 0.000000000000000000 ) ) ;
#15233 = CYLINDRICAL_SURFACE ( 'NONE', #2017, 12.00000000001200107 ) ;
#15234 = ORIENTED_EDGE ( 'NONE', *, *, #17820, .T. ) ;
#15235 = DIRECTION ( 'NONE',  ( -1.000000000000000000, 0.000000000000000000, 0.000000000000000000 ) ) ;
#15236 = EDGE_LOOP ( 'NONE', ( #9501, #18071, #13127, #18636 ) ) ;
#15237 = DIRECTION ( 'NONE',  ( -1.000000000000000000, -0.000000000000000000, 0.000000000000000000 ) ) ;
#15238 = CARTESIAN_POINT ( 'NONE',  ( 45.00000000000000000, 10.00000000000000000, -5.120903701083534543E-13 ) ) ;
#15239 = CIRCLE ( 'NONE', #1259, 24.00000000002400213 ) ;
#15240 = ADVANCED_FACE ( 'NONE', ( #6623 ), #14049, .F. ) ;
#15241 = EDGE_LOOP ( 'NONE', ( #3702, #7115, #16918, #1748 ) ) ;
#15242 = EDGE_CURVE ( 'NONE', #17667, #9474, #12325, .T. ) ;
#15243 = VERTEX_POINT ( 'NONE', #13761 ) ;
#15244 = DIRECTION ( 'NONE',  ( 0.000000000000000000, 0.000000000000000000, 1.000000000000000000 ) ) ;
#15245 = FACE_OUTER_BOUND ( 'NONE', #14469, .T. ) ;
#15246 = DIRECTION ( 'NONE',  ( 0.000000000000000000, 0.000000000000000000, 1.000000000000000000 ) ) ;
#15247 = DIRECTION ( 'NONE',  ( 0.000000000000000000, 0.000000000000000000, -1.000000000000000000 ) ) ;
#15248 = AXIS2_PLACEMENT_3D ( 'NONE', #7664, #6238, #1670 ) ;
#15249 = DIRECTION ( 'NONE',  ( 0.000000000000000000, 0.000000000000000000, 1.000000000000000000 ) ) ;
#15250 = DIRECTION ( 'NONE',  ( 0.000000000000000000, -0.5000000000000009992, -0.8660254037844380415 ) ) ;
#15251 = VERTEX_POINT ( 'NONE', #11185 ) ;
#15252 = DIRECTION ( 'NONE',  ( 0.000000000000000000, 0.3090169943749479509, -0.9510565162951533091 ) ) ;
#15253 = DIRECTION ( 'NONE',  ( -1.000000000000000000, 0.000000000000000000, 0.000000000000000000 ) ) ;
#15254 = ORIENTED_EDGE ( 'NONE', *, *, #18740, .T. ) ;
#15255 = ORIENTED_EDGE ( 'NONE', *, *, #12722, .F. ) ;
#15256 = AXIS2_PLACEMENT_3D ( 'NONE', #8520, #5487, #11284 ) ;
#15257 = EDGE_LOOP ( 'NONE', ( #4287, #11964, #5489, #10288 ) ) ;
#15258 = ORIENTED_EDGE ( 'NONE', *, *, #16640, .F. ) ;
#15259 = CARTESIAN_POINT ( 'NONE',  ( 10.00000000000000000, 0.000000000000000000, 0.000000000000000000 ) ) ;
#15260 = CARTESIAN_POINT ( 'NONE',  ( 0.000000000000000000, 0.000000000000000000, 0.000000000000000000 ) ) ;
#15261 = PLANE ( 'NONE',  #6268 ) ;
#15262 = FACE_BOUND ( 'NONE', #7734, .T. ) ;
#15263 = DIRECTION ( 'NONE',  ( -1.000000000000000000, 0.000000000000000000, -0.000000000000000000 ) ) ;
#15264 = VERTEX_POINT ( 'NONE', #18420 ) ;
#15265 = CARTESIAN_POINT ( 'NONE',  ( 5.000000000000000000, -40.19788616105574164, -48.50907078259425731 ) ) ;
#15266 = ORIENTED_EDGE ( 'NONE', *, *, #12907, .T. ) ;
#15267 = CARTESIAN_POINT ( 'NONE',  ( 10.00000000000000000, 45.00825343885021113, 33.95787273855260935 ) ) ;
#15268 = DIRECTION ( 'NONE',  ( 0.000000000000000000, 0.000000000000000000, 1.000000000000000000 ) ) ;
#15269 = VERTEX_POINT ( 'NONE', #17015 ) ;
#15270 = ORIENTED_EDGE ( 'NONE', *, *, #14263, .F. ) ;
#15271 = EDGE_CURVE ( 'NONE', #12788, #5391, #12392, .T. ) ;
#15272 = FACE_OUTER_BOUND ( 'NONE', #4880, .T. ) ;
#15273 = CARTESIAN_POINT ( 'NONE',  ( 13.90576474687263975, -14.99999999999999289, -42.79754323328191390 ) ) ;
#15274 = AXIS2_PLACEMENT_3D ( 'NONE', #18669, #9723, #18288 ) ;
#15276 = EDGE_CURVE ( 'NONE', #417, #8897, #17560, .T. ) ;
#15275 = CYLINDRICAL_SURFACE ( 'NONE', #10198, 24.00000000002399858 ) ;
#15277 = VERTEX_POINT ( 'NONE', #3676 ) ;
#15278 = EDGE_CURVE ( 'NONE', #7239, #3393, #10859, .T. ) ;
#15279 = EDGE_CURVE ( 'NONE', #8733, #15277, #2983, .T. ) ;
#15280 = FACE_OUTER_BOUND ( 'NONE', #5396, .T. ) ;
#15281 = CARTESIAN_POINT ( 'NONE',  ( 21.00000000000000355, 0.000000000000000000, 0.000000000000000000 ) ) ;
#15282 = LINE ( 'NONE', #6807, #1149 ) ;
#15283 = ORIENTED_EDGE ( 'NONE', *, *, #13975, .T. ) ;
#15284 = DIRECTION ( 'NONE',  ( 0.000000000000000000, 0.000000000000000000, 1.000000000000000000 ) ) ;
#15285 =( BOUNDED_SURFACE ( )  B_SPLINE_SURFACE ( 3, 2, ( 
 ( #13773, #440, #15115 ),
 ( #9195, #7585, #1959 ),
 ( #16536, #11962, #352 ),
 ( #13408, #6442, #544 ),
 ( #6153, #12245, #6246 ),
 ( #17769, #12054, #16254 ) ),
 .UNSPECIFIED., .F., .F., .T. ) 
 B_SPLINE_SURFACE_WITH_KNOTS ( ( 4, 2, 4 ),
 ( 3, 3 ),
 ( 0.02032853247518125531, 0.02278863295364820865, 0.02524873343211516200 ),
 ( 0.000000000000000000, 1.000000000000000000 ),
 .UNSPECIFIED. ) 
 GEOMETRIC_REPRESENTATION_ITEM ( )  RATIONAL_B_SPLINE_SURFACE ( (
 ( 1.000000000000000000, 0.8047781615896836271, 1.000000000000000000),
 ( 1.000000000000000000, 0.8123767586289967202, 1.000000000000000000),
 ( 1.000000000000000000, 0.8190662415563443322, 1.000000000000000000),
 ( 1.000000000000000000, 0.8192361015669982205, 1.000000000000000000),
 ( 1.000000000000000000, 0.8126135807103181952, 1.000000000000000000),
 ( 1.000000000000000000, 0.8047712338318587788, 1.000000000000000000) ) ) 
 REPRESENTATION_ITEM ( '' )  SURFACE ( )  );
#15286 = CIRCLE ( 'NONE', #2513, 6.080745460913608902 ) ;
#15287 = EDGE_CURVE ( 'NONE', #12513, #18363, #8338, .T. ) ;
#15288 = CIRCLE ( 'NONE', #1903, 12.00000000001200284 ) ;
#15289 = ORIENTED_EDGE ( 'NONE', *, *, #10975, .T. ) ;
#15290 = UNCERTAINTY_MEASURE_WITH_UNIT (LENGTH_MEASURE( 1.000000000000000082E-05 ), #14683, 'distance_accuracy_value', 'NONE');
#15291 = FACE_OUTER_BOUND ( 'NONE', #13855, .T. ) ;
#15292 = EDGE_LOOP ( 'NONE', ( #13732, #4596, #11543, #9288 ) ) ;
#15293 = DIRECTION ( 'NONE',  ( -1.000000000000000000, 0.000000000000000000, 0.000000000000000000 ) ) ;
#15294 = CARTESIAN_POINT ( 'NONE',  ( 10.00000000000000000, 15.61693798565582902, -61.03368945066418405 ) ) ;
#15295 = DIRECTION ( 'NONE',  ( 1.000000000000000000, 0.000000000000000000, 0.000000000000000000 ) ) ;
#15296 = ORIENTED_EDGE ( 'NONE', *, *, #10055, .T. ) ;
#15297 = EDGE_LOOP ( 'NONE', ( #15627, #1174, #10201, #15835 ) ) ;
#15298 = EDGE_CURVE ( 'NONE', #5739, #18350, #2613, .T. ) ;
#15299 = CARTESIAN_POINT ( 'NONE',  ( 10.00000000000000000, 0.000000000000000000, 0.000000000000000000 ) ) ;
#15300 = EDGE_CURVE ( 'NONE', #18412, #645, #15282, .T. ) ;
#15301 = ORIENTED_EDGE ( 'NONE', *, *, #16180, .F. ) ;
#15302 = CARTESIAN_POINT ( 'NONE',  ( 0.000000000000000000, 13.24999999999999822, 25.00000000000000000 ) ) ;
#15303 = AXIS2_PLACEMENT_3D ( 'NONE', #4721, #6353, #10533 ) ;
#15304 = ADVANCED_FACE ( 'NONE', ( #12716 ), #6518, .T. ) ;
#15305 = CIRCLE ( 'NONE', #14689, 24.00000000002399858 ) ;
#15306 = EDGE_CURVE ( 'NONE', #9474, #4599, #13310, .T. ) ;
#15307 = LINE ( 'NONE', #15591, #10790 ) ;
#15308 = DIRECTION ( 'NONE',  ( 0.000000000000000000, -1.000000000000000000, 0.000000000000000000 ) ) ;
#15309 = EDGE_LOOP ( 'NONE', ( #15400, #1574 ) ) ;
#15310 = ORIENTED_EDGE ( 'NONE', *, *, #15871, .T. ) ;
#15311 = CARTESIAN_POINT ( 'NONE',  ( 10.00000000000000000, 0.000000000000000000, 0.000000000000000000 ) ) ;
#15312 = CARTESIAN_POINT ( 'NONE',  ( 10.00000000000000000, 32.31183295104839459, -46.20417134726096009 ) ) ;
#15313 = CARTESIAN_POINT ( 'NONE',  ( 10.00000000000000000, -44.70888270294135936, -34.13306034420235591 ) ) ;
#15314 = ORIENTED_EDGE ( 'NONE', *, *, #10959, .T. ) ;
#15315 = CYLINDRICAL_SURFACE ( 'NONE', #6074, 12.00000000001200284 ) ;
#15316 = ORIENTED_EDGE ( 'NONE', *, *, #8537, .F. ) ;
#15317 = VECTOR ( 'NONE', #4336, 1000.000000000000000 ) ;
#15318 = CARTESIAN_POINT ( 'NONE',  ( 2.500000000000000000, 0.000000000000000000, 2.041999999999999815 ) ) ;
#15319 = PLANE ( 'NONE',  #9509 ) ;
#15320 = VERTEX_POINT ( 'NONE', #16727 ) ;
#15321 = VERTEX_POINT ( 'NONE', #10899 ) ;
#15322 = LINE ( 'NONE', #169, #12324 ) ;
#15323 = EDGE_LOOP ( 'NONE', ( #12491, #16910 ) ) ;
#15324 = DIRECTION ( 'NONE',  ( 0.000000000000000000, 1.000000000000000000, 0.000000000000000000 ) ) ;
#15325 = CARTESIAN_POINT ( 'NONE',  ( 0.000000000000000000, -56.37237871411034718, 1.017308535512174261 ) ) ;
#15326 = EDGE_CURVE ( 'NONE', #15019, #12930, #6333, .T. ) ;
#15327 = ORIENTED_EDGE ( 'NONE', *, *, #3479, .T. ) ;
#15328 = ORIENTED_EDGE ( 'NONE', *, *, #9114, .F. ) ;
#15329 = DIRECTION ( 'NONE',  ( 0.000000000000000000, 0.000000000000000000, 1.000000000000000000 ) ) ;
#15330 = CARTESIAN_POINT ( 'NONE',  ( 4.000000000000000000, -0.8732470631449981147, -3.223155494240760088 ) ) ;
#15331 = FACE_OUTER_BOUND ( 'NONE', #334, .T. ) ;
#15332 = DIRECTION ( 'NONE',  ( 0.000000000000000000, 0.000000000000000000, -1.000000000000000000 ) ) ;
#15333 = DIRECTION ( 'NONE',  ( -1.000000000000000000, 0.000000000000000000, 0.000000000000000000 ) ) ;
#15334 = LINE ( 'NONE', #15058, #3218 ) ;
#15335 = ORIENTED_EDGE ( 'NONE', *, *, #6742, .F. ) ;
#15336 = DIRECTION ( 'NONE',  ( -1.000000000000000000, -0.000000000000000000, 0.000000000000000000 ) ) ;
#15337 = CARTESIAN_POINT ( 'NONE',  ( 10.00000000000000000, -22.07705612348849655, 14.19907017806860949 ) ) ;
#15338 = CARTESIAN_POINT ( 'NONE',  ( 10.00000000000000000, 55.83748330407408389, 16.18620087215052195 ) ) ;
#15339 = EDGE_CURVE ( 'NONE', #4921, #7351, #16367, .T. ) ;
#15340 = EDGE_LOOP ( 'NONE', ( #10278, #4973 ) ) ;
#15341 = ORIENTED_EDGE ( 'NONE', *, *, #4124, .T. ) ;
#15342 = VERTEX_POINT ( 'NONE', #16904 ) ;
#15343 = AXIS2_PLACEMENT_3D ( 'NONE', #11947, #617, #7654 ) ;
#15344 = DIRECTION ( 'NONE',  ( 0.000000000000000000, 0.000000000000000000, 1.000000000000000000 ) ) ;
#15345 = LINE ( 'NONE', #2497, #13702 ) ;
#15346 = SURFACE_STYLE_USAGE ( .BOTH. , #2498 ) ;
#15347 = VECTOR ( 'NONE', #11973, 1000.000000000000000 ) ;
#15348 = CARTESIAN_POINT ( 'NONE',  ( 10.00000000000000000, -15.61693798565540625, 61.03368945066429774 ) ) ;
#15349 = LINE ( 'NONE', #13654, #10032 ) ;
#15350 = FACE_OUTER_BOUND ( 'NONE', #3083, .T. ) ;
#15351 = DIRECTION ( 'NONE',  ( -1.000000000000000000, 0.000000000000000000, 0.000000000000000000 ) ) ;
#15352 = DIRECTION ( 'NONE',  ( -1.000000000000000000, 0.000000000000000000, 0.000000000000000000 ) ) ;
#15353 = VERTEX_POINT ( 'NONE', #2329 ) ;
#15354 = CARTESIAN_POINT ( 'NONE',  ( -36.40576474687271258, 0.000000000000000000, -29.10033635316118961 ) ) ;
#15355 = ORIENTED_EDGE ( 'NONE', *, *, #8875, .F. ) ;
#15356 = EDGE_CURVE ( 'NONE', #5321, #6583, #2231, .T. ) ;
#15357 = EDGE_CURVE ( 'NONE', #13630, #16495, #3291, .T. ) ;
#15358 = DIRECTION ( 'NONE',  ( -1.000000000000000000, 0.000000000000000000, 0.000000000000000000 ) ) ;
#15359 = DIRECTION ( 'NONE',  ( 0.000000000000000000, 0.000000000000000000, 1.000000000000000000 ) ) ;
#15360 = ORIENTED_EDGE ( 'NONE', *, *, #1967, .T. ) ;
#15361 = ORIENTED_EDGE ( 'NONE', *, *, #10266, .T. ) ;
#15362 = DIRECTION ( 'NONE',  ( 0.000000000000000000, 0.4999999999999992784, -0.8660254037844390407 ) ) ;
#15363 = DIRECTION ( 'NONE',  ( -0.6837499115219671797, 7.285838599102589797E-17, 0.7297164233410826650 ) ) ;
#15364 = EDGE_CURVE ( 'NONE', #4661, #298, #16987, .T. ) ;
#15365 = DIRECTION ( 'NONE',  ( 0.000000000000000000, 0.000000000000000000, 1.000000000000000000 ) ) ;
#15366 = CARTESIAN_POINT ( 'NONE',  ( 0.000000000000000000, 24.68609584167230153, -50.69000562871616467 ) ) ;
#15367 = ORIENTED_EDGE ( 'NONE', *, *, #8334, .F. ) ;
#15368 = CIRCLE ( 'NONE', #11413, 33.00000000003299760 ) ;
#15369 = VECTOR ( 'NONE', #12505, 1000.000000000000000 ) ;
#15370 = CARTESIAN_POINT ( 'NONE',  ( 10.00000000000000000, 32.31183295104772668, 46.20417134726143615 ) ) ;
#15371 = FACE_BOUND ( 'NONE', #12550, .T. ) ;
#15372 = CIRCLE ( 'NONE', #11118, 12.00000000001200640 ) ;
#15373 = CARTESIAN_POINT ( 'NONE',  ( 2.250000000000000000, -27.60846790388774608, -2.000000000000000000 ) ) ;
#15374 = ORIENTED_EDGE ( 'NONE', *, *, #7805, .T. ) ;
#15375 = DIRECTION ( 'NONE',  ( 0.000000000000000000, -0.9510565162951502005, -0.3090169943749581649 ) ) ;
#15376 = ADVANCED_FACE ( 'NONE', ( #13956 ), #18329, .F. ) ;
#15377 = VECTOR ( 'NONE', #15872, 1000.000000000000000 ) ;
#15378 = ORIENTED_EDGE ( 'NONE', *, *, #3307, .F. ) ;
#15379 = DIRECTION ( 'NONE',  ( -1.000000000000000000, -0.000000000000000000, -0.000000000000000000 ) ) ;
#15380 = AXIS2_PLACEMENT_3D ( 'NONE', #11831, #17640, #12386 ) ;
#15381 = EDGE_LOOP ( 'NONE', ( #3768, #14405, #156, #12532 ) ) ;
#15382 = PRODUCT_DEFINITION ( 'UNKNOWN', '', #12941, #6933 ) ;
#15383 = CARTESIAN_POINT ( 'NONE',  ( 0.3198814748697593746, 4.434118497892183264, -0.3507732604232499107 ) ) ;
#15384 = CARTESIAN_POINT ( 'NONE',  ( 12.49999999999999289, 0.000000000000000000, 0.000000000000000000 ) ) ;
#15385 = DIRECTION ( 'NONE',  ( -0.000000000000000000, 1.000000000000000000, -0.000000000000000000 ) ) ;
#15386 = ORIENTED_EDGE ( 'NONE', *, *, #274, .T. ) ;
#15387 = ORIENTED_EDGE ( 'NONE', *, *, #10342, .T. ) ;
#15388 = CARTESIAN_POINT ( 'NONE',  ( 0.000000000000000000, 5.086963483077203918, 27.72801475327284138 ) ) ;
#15389 = ORIENTED_EDGE ( 'NONE', *, *, #7615, .F. ) ;
#15390 = CARTESIAN_POINT ( 'NONE',  ( 5.000000000000000000, 23.88582760061514421, -22.76987570971501640 ) ) ;
#15391 = AXIS2_PLACEMENT_3D ( 'NONE', #4636, #11876, #4920 ) ;
#15392 = AXIS2_PLACEMENT_3D ( 'NONE', #12778, #4107, #7842 ) ;
#15393 = AXIS2_PLACEMENT_3D ( 'NONE', #9638, #15459, #11908 ) ;
#15394 = CIRCLE ( 'NONE', #3232, 63.00000000006298961 ) ;
#15395 = VECTOR ( 'NONE', #13211, 1000.000000000000000 ) ;
#15396 = AXIS2_PLACEMENT_3D ( 'NONE', #16185, #13428, #8846 ) ;
#15397 = CARTESIAN_POINT ( 'NONE',  ( -6.259644161404860030E-16, -4.618802153517027165, -5.000000000000000000 ) ) ;
#15398 = CARTESIAN_POINT ( 'NONE',  ( -26.29305231718568336, -30.00000000000000000, -19.10302069950552095 ) ) ;
#15399 = EDGE_CURVE ( 'NONE', #192, #1880, #12713, .T. ) ;
#15400 = ORIENTED_EDGE ( 'NONE', *, *, #12876, .T. ) ;
#15401 = EDGE_CURVE ( 'NONE', #18678, #4356, #9350, .T. ) ;
#15402 = FILL_AREA_STYLE_COLOUR ( '', #9146 ) ;
#15403 = EDGE_CURVE ( 'NONE', #13362, #9382, #7854, .T. ) ;
#15404 = EDGE_CURVE ( 'NONE', #451, #12684, #13024, .T. ) ;
#15405 = VECTOR ( 'NONE', #9268, 1000.000000000000000 ) ;
#15406 = ORIENTED_EDGE ( 'NONE', *, *, #18085, .T. ) ;
#15407 = DIRECTION ( 'NONE',  ( 0.000000000000000000, 0.000000000000000000, 1.000000000000000000 ) ) ;
#15408 = CYLINDRICAL_SURFACE ( 'NONE', #7437, 56.24900000005625600 ) ;
#15410 = CIRCLE ( 'NONE', #10242, 12.00000000001200462 ) ;
#15409 = CYLINDRICAL_SURFACE ( 'NONE', #11498, 8.099999999999999645 ) ;
#15411 = ORIENTED_EDGE ( 'NONE', *, *, #729, .T. ) ;
#15412 = LINE ( 'NONE', #8178, #10548 ) ;
#15413 = ORIENTED_EDGE ( 'NONE', *, *, #3309, .F. ) ;
#15414 = AXIS2_PLACEMENT_3D ( 'NONE', #9429, #16485, #3442 ) ;
#15415 = EDGE_CURVE ( 'NONE', #16428, #10912, #12726, .T. ) ;
#15416 = FACE_OUTER_BOUND ( 'NONE', #12823, .T. ) ;
#15417 = CARTESIAN_POINT ( 'NONE',  ( 0.000000000000000000, 53.06836994729233936, 18.64666490672390964 ) ) ;
#15418 = VECTOR ( 'NONE', #11155, 1000.000000000000000 ) ;
#15419 = ORIENTED_EDGE ( 'NONE', *, *, #15061, .F. ) ;
#15420 = VERTEX_POINT ( 'NONE', #1561 ) ;
#15421 = AXIS2_PLACEMENT_3D ( 'NONE', #7908, #16861, #6480 ) ;
#15422 =( NAMED_UNIT ( * ) PLANE_ANGLE_UNIT ( ) SI_UNIT ( $, .RADIAN. ) );
#15423 = ORIENTED_EDGE ( 'NONE', *, *, #717, .F. ) ;
#15424 = CARTESIAN_POINT ( 'NONE',  ( 0.2500000000000002220, 0.000000000000000000, 4.000000000000000000 ) ) ;
#15425 = LINE ( 'NONE', #3800, #5225 ) ;
#15426 = EDGE_CURVE ( 'NONE', #2263, #4897, #17380, .T. ) ;
#15427 = CIRCLE ( 'NONE', #9318, 2.649999999999999467 ) ;
#15428 = CIRCLE ( 'NONE', #1439, 5.000000000000000000 ) ;
#15429 = CIRCLE ( 'NONE', #18775, 12.00000000001200817 ) ;
#15430 = ORIENTED_EDGE ( 'NONE', *, *, #5976, .F. ) ;
#15431 = EDGE_CURVE ( 'NONE', #7464, #10253, #18616, .T. ) ;
#15432 = VERTEX_POINT ( 'NONE', #2716 ) ;
#15433 = DIRECTION ( 'NONE',  ( -1.000000000000000000, 0.000000000000000000, 0.000000000000000000 ) ) ;
#15434 = DIRECTION ( 'NONE',  ( 0.000000000000000000, 0.000000000000000000, 1.000000000000000000 ) ) ;
#15435 = CARTESIAN_POINT ( 'NONE',  ( 10.00000000000000000, 0.000000000000000000, 0.000000000000000000 ) ) ;
#15436 = DIRECTION ( 'NONE',  ( -1.000000000000000000, 0.000000000000000000, 0.000000000000000000 ) ) ;
#15437 = LINE ( 'NONE', #12870, #16190 ) ;
#15438 = CIRCLE ( 'NONE', #3870, 56.24900000005625600 ) ;
#15439 = DIRECTION ( 'NONE',  ( 0.000000000000000000, 1.000000000000000000, 0.000000000000000000 ) ) ;
#15440 = ORIENTED_EDGE ( 'NONE', *, *, #3280, .T. ) ;
#15441 = CARTESIAN_POINT ( 'NONE',  ( 10.00000000000000000, 0.000000000000000000, 0.000000000000000000 ) ) ;
#15442 = EDGE_CURVE ( 'NONE', #16873, #3875, #17562, .T. ) ;
#15443 = CYLINDRICAL_SURFACE ( 'NONE', #5945, 56.24900000005625600 ) ;
#15444 = AXIS2_PLACEMENT_3D ( 'NONE', #10334, #16427, #17847 ) ;
#15445 = CARTESIAN_POINT ( 'NONE',  ( 0.000000000000000000, 26.71881558261799228, -49.49802920186195365 ) ) ;
#15446 = CARTESIAN_POINT ( 'NONE',  ( 0.000000000000000000, -26.50000000000000000, -41.00000000000000000 ) ) ;
#15447 = CIRCLE ( 'NONE', #14221, 56.24900000005625600 ) ;
#15448 = AXIS2_PLACEMENT_3D ( 'NONE', #4125, #2695, #2303 ) ;
#15449 = ITEM_DEFINED_TRANSFORMATION ( 'NONE', 'NONE', #9565,  #8017 ) ;
#15450 = ORIENTED_EDGE ( 'NONE', *, *, #868, .F. ) ;
#15451 = ORIENTED_EDGE ( 'NONE', *, *, #6214, .T. ) ;
#15452 = AXIS2_PLACEMENT_3D ( 'NONE', #8272, #12353, #3701 ) ;
#15453 = ORIENTED_EDGE ( 'NONE', *, *, #11450, .T. ) ;
#15454 = AXIS2_PLACEMENT_3D ( 'NONE', #18102, #18382, #14015 ) ;
#15455 = LINE ( 'NONE', #2405, #13600 ) ;
#15456 = CYLINDRICAL_SURFACE ( 'NONE', #17964, 24.00000000002399858 ) ;
#15457 = VECTOR ( 'NONE', #15333, 1000.000000000000000 ) ;
#15458 = DIRECTION ( 'NONE',  ( 0.000000000000000000, -1.000000000000000000, 0.000000000000000000 ) ) ;
#15459 = DIRECTION ( 'NONE',  ( 1.000000000000000000, 0.000000000000000000, 0.000000000000000000 ) ) ;
#15460 = DIRECTION ( 'NONE',  ( 0.000000000000000000, 0.000000000000000000, 1.000000000000000000 ) ) ;
#15461 = CARTESIAN_POINT ( 'NONE',  ( 0.000000000000000000, 54.20017844242511273, 32.11449294037214486 ) ) ;
#15462 = DIRECTION ( 'NONE',  ( -1.000000000000000000, 0.000000000000000000, 0.000000000000000000 ) ) ;
#15463 = CARTESIAN_POINT ( 'NONE',  ( 10.00000000000000000, -18.38754094778278869, 53.29895248911668659 ) ) ;
#15464 = VERTEX_POINT ( 'NONE', #14512 ) ;
#15465 = CARTESIAN_POINT ( 'NONE',  ( 11.25000000000000000, 29.90000000000000213, 0.000000000000000000 ) ) ;
#15466 = ORIENTED_EDGE ( 'NONE', *, *, #5026, .T. ) ;
#15467 = EDGE_CURVE ( 'NONE', #858, #202, #10291, .T. ) ;
#15468 = DIRECTION ( 'NONE',  ( 0.000000000000000000, 0.000000000000000000, 1.000000000000000000 ) ) ;
#15469 = DIRECTION ( 'NONE',  ( 0.000000000000000000, 1.000000000000000000, 0.000000000000000000 ) ) ;
#15470 = CONICAL_SURFACE ( 'NONE', #10885, 2.041999999999999815, 1.047197551196591858 ) ;
#15471 = EDGE_LOOP ( 'NONE', ( #2526, #10650, #6247, #2215 ) ) ;
#15472 = ORIENTED_EDGE ( 'NONE', *, *, #3601, .T. ) ;
#15473 = CARTESIAN_POINT ( 'NONE',  ( 10.00000000000000000, -13.40641754777648487, -24.79895094899273644 ) ) ;
#15474 = DIRECTION ( 'NONE',  ( -0.8090169943749507819, 6.123233995736766036E-17, 0.5877852522924685852 ) ) ;
#15475 = DIRECTION ( 'NONE',  ( -1.000000000000000000, -0.000000000000000000, -0.000000000000000000 ) ) ;
#15476 = EDGE_LOOP ( 'NONE', ( #13619, #9942 ) ) ;
#15477 = VECTOR ( 'NONE', #8570, 1000.000000000000000 ) ;
#15478 = EDGE_CURVE ( 'NONE', #1304, #726, #17291, .T. ) ;
#15479 = DIRECTION ( 'NONE',  ( 0.000000000000000000, 0.3090169943749411785, 0.9510565162951556406 ) ) ;
#15480 = CARTESIAN_POINT ( 'NONE',  ( 4.204015924366189871, -1.626724848190933548, -3.610627190413393084 ) ) ;
#15481 = CIRCLE ( 'NONE', #4837, 30.00000000000000711 ) ;
#15482 = DIRECTION ( 'NONE',  ( 0.000000000000000000, 0.000000000000000000, -1.000000000000000000 ) ) ;
#15483 = DIRECTION ( 'NONE',  ( 0.04803802292983955224, 0.000000000000000000, -0.9988455077503187729 ) ) ;
#15484 = EDGE_CURVE ( 'NONE', #6555, #11633, #9672, .T. ) ;
#15485 = ORIENTED_EDGE ( 'NONE', *, *, #6156, .F. ) ;
#15486 = UNCERTAINTY_MEASURE_WITH_UNIT (LENGTH_MEASURE( 1.000000000000000082E-05 ), #4476, 'distance_accuracy_value', 'NONE');
#15487 = CARTESIAN_POINT ( 'NONE',  ( -117.1020693116506379, -34.99999999999999289, -17.04080595179801705 ) ) ;
#15488 = ORIENTED_EDGE ( 'NONE', *, *, #3198, .F. ) ;
#15489 = DIRECTION ( 'NONE',  ( -1.000000000000000000, -0.000000000000000000, -0.000000000000000000 ) ) ;
#15490 = CARTESIAN_POINT ( 'NONE',  ( 5.000000000000000000, -33.71303790549312396, 53.22058882792185841 ) ) ;
#15491 = DIRECTION ( 'NONE',  ( -1.000000000000000000, -0.000000000000000000, 0.000000000000000000 ) ) ;
#15492 = ORIENTED_EDGE ( 'NONE', *, *, #13156, .F. ) ;
#15493 = EDGE_LOOP ( 'NONE', ( #6653, #7783, #3619, #11548 ) ) ;
#15494 = CARTESIAN_POINT ( 'NONE',  ( -117.1020693116508085, -34.99999999999999289, 22.34080595179777262 ) ) ;
#15495 = EDGE_LOOP ( 'NONE', ( #18344, #18016, #7398, #17256 ) ) ;
#15496 = CARTESIAN_POINT ( 'NONE',  ( 34.99999999999999289, 2.789133085058097101E-16, -2.055000000000000160 ) ) ;
#15497 = CIRCLE ( 'NONE', #15184, 4.250000000000000000 ) ;
#15498 = CIRCLE ( 'NONE', #7879, 2.649999999999999467 ) ;
#15499 = DIRECTION ( 'NONE',  ( -1.000000000000000000, 0.000000000000000000, 0.000000000000000000 ) ) ;
#15500 = DIRECTION ( 'NONE',  ( 0.000000000000000000, 0.9510565162951543083, -0.3090169943749447312 ) ) ;
#15501 = ORIENTED_EDGE ( 'NONE', *, *, #9369, .F. ) ;
#15502 = LINE ( 'NONE', #1994, #5814 ) ;
#15503 = AXIS2_PLACEMENT_3D ( 'NONE', #18536, #2440, #16825 ) ;
#15504 = EDGE_LOOP ( 'NONE', ( #16385, #14606 ) ) ;
#15505 = DIRECTION ( 'NONE',  ( 1.000000000000000000, 0.000000000000000000, 0.000000000000000000 ) ) ;
#15506 = DIRECTION ( 'NONE',  ( -1.000000000000000000, -0.000000000000000000, -0.000000000000000000 ) ) ;
#15507 = CARTESIAN_POINT ( 'NONE',  ( 10.00000000000000000, 0.000000000000000000, 0.000000000000000000 ) ) ;
#15508 = ORIENTED_EDGE ( 'NONE', *, *, #16460, .F. ) ;
#15509 = CARTESIAN_POINT ( 'NONE',  ( -1.128893538851230005, 11.24999999999999467, 23.47286943213250154 ) ) ;
#15510 = ORIENTED_EDGE ( 'NONE', *, *, #14134, .F. ) ;
#15511 = DIRECTION ( 'NONE',  ( 1.000000000000000000, 0.000000000000000000, 0.000000000000000000 ) ) ;
#15512 = DIRECTION ( 'NONE',  ( -1.000000000000000000, -0.000000000000000000, -0.000000000000000000 ) ) ;
#15513 = EDGE_LOOP ( 'NONE', ( #6659, #9346, #3933, #6090 ) ) ;
#15514 = EDGE_LOOP ( 'NONE', ( #287, #10911, #5655, #12315 ) ) ;
#15515 = DIRECTION ( 'NONE',  ( -1.000000000000000000, 0.000000000000000000, -0.000000000000000000 ) ) ;
#15516 = ORIENTED_EDGE ( 'NONE', *, *, #17692, .T. ) ;
#15517 = DIRECTION ( 'NONE',  ( -1.000000000000000000, 0.000000000000000000, 0.000000000000000000 ) ) ;
#15518 = DIRECTION ( 'NONE',  ( 0.000000000000000000, 0.8090169943749486725, -0.5877852522924712497 ) ) ;
#15519 = EDGE_CURVE ( 'NONE', #5833, #10254, #13322, .T. ) ;
#15520 = ADVANCED_FACE ( 'NONE', ( #2999 ), #14418, .T. ) ;
#15521 = EDGE_CURVE ( 'NONE', #2269, #11877, #4411, .T. ) ;
#15522 = AXIS2_PLACEMENT_3D ( 'NONE', #18713, #4524, #144 ) ;
#15523 = AXIS2_PLACEMENT_3D ( 'NONE', #16902, #18417, #18526 ) ;
#15524 = EDGE_CURVE ( 'NONE', #1965, #18064, #11797, .T. ) ;
#15525 = EDGE_LOOP ( 'NONE', ( #6986, #15141, #17171, #10531 ) ) ;
#15526 = ADVANCED_FACE ( 'NONE', ( #14609 ), #1290, .T. ) ;
#15527 = ORIENTED_EDGE ( 'NONE', *, *, #10293, .F. ) ;
#15528 = FACE_OUTER_BOUND ( 'NONE', #3005, .T. ) ;
#15529 = CARTESIAN_POINT ( 'NONE',  ( -4.000000000000000000, 2.309401076758498483, -0.4999999999999927280 ) ) ;
#15530 = DIRECTION ( 'NONE',  ( -1.000000000000000000, 0.000000000000000000, 0.000000000000000000 ) ) ;
#15531 = CYLINDRICAL_SURFACE ( 'NONE', #17548, 2.649999999999999467 ) ;
#15532 = EDGE_CURVE ( 'NONE', #262, #5512, #1375, .T. ) ;
#15533 = DIRECTION ( 'NONE',  ( -1.000000000000000000, -0.000000000000000000, 0.000000000000000000 ) ) ;
#15534 = DIRECTION ( 'NONE',  ( 1.000000000000000000, 0.000000000000000000, 0.000000000000000000 ) ) ;
#15535 = DIRECTION ( 'NONE',  ( 0.000000000000000000, 1.000000000000000000, 0.000000000000000000 ) ) ;
#15536 = VERTEX_POINT ( 'NONE', #11749 ) ;
#15537 = DIRECTION ( 'NONE',  ( 0.000000000000000000, 0.000000000000000000, 1.000000000000000000 ) ) ;
#15538 = DIRECTION ( 'NONE',  ( 0.000000000000000000, 0.5877852522924742473, -0.8090169943749465631 ) ) ;
#15539 = DIRECTION ( 'NONE',  ( -1.000000000000000000, 0.000000000000000000, 0.000000000000000000 ) ) ;
#15540 = CARTESIAN_POINT ( 'NONE',  ( 10.00000000000000000, -26.71881558261695133, -49.49802920186252209 ) ) ;
#15541 = EDGE_CURVE ( 'NONE', #407, #13852, #869, .T. ) ;
#15542 = ITEM_DEFINED_TRANSFORMATION ( 'NONE', 'NONE', #14155,  #8017 ) ;
#15543 = EDGE_CURVE ( 'NONE', #11178, #2985, #3594, .T. ) ;
#15544 = ORIENTED_EDGE ( 'NONE', *, *, #9480, .T. ) ;
#15545 = ORIENTED_EDGE ( 'NONE', *, *, #1432, .T. ) ;
#15546 = ADVANCED_FACE ( 'NONE', ( #13652 ), #7832, .F. ) ;
#15547 = EDGE_LOOP ( 'NONE', ( #5215, #3977, #12546, #4830 ) ) ;
#15548 = AXIS2_PLACEMENT_3D ( 'NONE', #4268, #17128, #15876 ) ;
#15549 = CARTESIAN_POINT ( 'NONE',  ( 0.000000000000000000, -32.70783759231083820, -4.381479206523335890 ) ) ;
#15550 = CARTESIAN_POINT ( 'NONE',  ( 0.000000000000000000, -30.00000000000000000, 0.000000000000000000 ) ) ;
#15551 = DIRECTION ( 'NONE',  ( 0.000000000000000000, -0.8910065241883721177, 0.4539904997395383113 ) ) ;
#15552 = CARTESIAN_POINT ( 'NONE',  ( 10.00000000000000000, 9.514709542736897063, 24.46385708179987262 ) ) ;
#15553 = DIRECTION ( 'NONE',  ( -0.000000000000000000, 1.000000000000000000, -0.000000000000000000 ) ) ;
#15554 = CARTESIAN_POINT ( 'NONE',  ( -90.00000000009001155, -10.00000000000001776, -1.301042606982605912E-15 ) ) ;
#15555 = DIRECTION ( 'NONE',  ( -1.000000000000000000, -0.000000000000000000, 0.000000000000000000 ) ) ;
#15556 = DIRECTION ( 'NONE',  ( 0.000000000000000000, 1.000000000000000000, 0.000000000000000000 ) ) ;
#15557 = ORIENTED_EDGE ( 'NONE', *, *, #174, .F. ) ;
#15558 = CARTESIAN_POINT ( 'NONE',  ( 0.000000000000000000, 0.000000000000000000, 0.000000000000000000 ) ) ;
#15559 = VERTEX_POINT ( 'NONE', #12118 ) ;
#15560 = CARTESIAN_POINT ( 'NONE',  ( -82.50000000008999734, -13.00000000000001954, -7.728702897168715310E-16 ) ) ;
#15561 = DIRECTION ( 'NONE',  ( -0.000000000000000000, -0.000000000000000000, -1.000000000000000000 ) ) ;
#15562 = ORIENTED_EDGE ( 'NONE', *, *, #7422, .F. ) ;
#15563 = CARTESIAN_POINT ( 'NONE',  ( 1.567478505476134606E-15, 4.618802153517012066, -5.000000000000000000 ) ) ;
#15564 = CIRCLE ( 'NONE', #2476, 29.90000000000000213 ) ;
#15565 = DIRECTION ( 'NONE',  ( 6.123233995736766036E-17, -1.000000000000000000, 0.000000000000000000 ) ) ;
#15566 = CARTESIAN_POINT ( 'NONE',  ( 10.00000000000000000, -22.76987570971509456, -23.88582760061506249 ) ) ;
#15567 = ORIENTED_EDGE ( 'NONE', *, *, #9369, .T. ) ;
#15568 = AXIS2_PLACEMENT_3D ( 'NONE', #18790, #11641, #6984 ) ;
#15569 = EDGE_CURVE ( 'NONE', #11858, #6887, #9973, .T. ) ;
#15570 = DIRECTION ( 'NONE',  ( 0.000000000000000000, 0.8090169943749486725, -0.5877852522924712497 ) ) ;
#15571 = CARTESIAN_POINT ( 'NONE',  ( 4.197393957002303999, 7.772902908466098641E-14, -3.503767560748929810 ) ) ;
#15572 = CARTESIAN_POINT ( 'NONE',  ( 0.000000000000000000, 1.305124410222461284, -2.000000000000000000 ) ) ;
#15573 = DIRECTION ( 'NONE',  ( 0.000000000000000000, 0.000000000000000000, 1.000000000000000000 ) ) ;
#15574 = CIRCLE ( 'NONE', #14647, 12.00000000001200640 ) ;
#15575 = LINE ( 'NONE', #924, #16062 ) ;
#15576 = ORIENTED_EDGE ( 'NONE', *, *, #2615, .T. ) ;
#15577 = CIRCLE ( 'NONE', #14966, 2.041999999999999815 ) ;
#15578 = CARTESIAN_POINT ( 'NONE',  ( 0.000000000000000000, -22.07705612348829050, -14.19907017806892924 ) ) ;
#15579 = LINE ( 'NONE', #18339, #10721 ) ;
#15580 = DIRECTION ( 'NONE',  ( -1.000000000000000000, 0.000000000000000000, 0.000000000000000000 ) ) ;
#15581 = ORIENTED_EDGE ( 'NONE', *, *, #4579, .F. ) ;
#15582 = ORIENTED_EDGE ( 'NONE', *, *, #18327, .T. ) ;
#15583 = CARTESIAN_POINT ( 'NONE',  ( 2.500000000000000000, -1.178949249685213863, 2.042000000000001148 ) ) ;
#15584 =( NAMED_UNIT ( * ) PLANE_ANGLE_UNIT ( ) SI_UNIT ( $, .RADIAN. ) );
#15585 = EDGE_CURVE ( 'NONE', #1536, #5770, #1759, .T. ) ;
#15586 = ORIENTED_EDGE ( 'NONE', *, *, #16180, .T. ) ;
#15587 = CARTESIAN_POINT ( 'NONE',  ( -117.1020693116506379, -34.99999999999999289, -19.69080595179801207 ) ) ;
#15588 = EDGE_CURVE ( 'NONE', #15536, #11085, #5101, .T. ) ;
#15589 = PRODUCT ( 'MAS-191', 'MAS-191', '', ( #4323 ) ) ;
#15590 = AXIS2_PLACEMENT_3D ( 'NONE', #3707, #12182, #3338 ) ;
#15591 = CARTESIAN_POINT ( 'NONE',  ( 5.000000000000000000, -23.24033432160480217, 58.55669782892453412 ) ) ;
#15592 = LINE ( 'NONE', #15683, #4778 ) ;
#15593 =( REPRESENTATION_RELATIONSHIP ('NONE','NONE', #11014, #2517 ) REPRESENTATION_RELATIONSHIP_WITH_TRANSFORMATION ( #18491 )SHAPE_REPRESENTATION_RELATIONSHIP( ) );
#15594 = VERTEX_POINT ( 'NONE', #14983 ) ;
#15595 = LINE ( 'NONE', #8628, #18279 ) ;
#15596 = VERTEX_POINT ( 'NONE', #10683 ) ;
#15597 = CARTESIAN_POINT ( 'NONE',  ( 0.000000000000000000, -32.11449294037235802, 54.20017844242499905 ) ) ;
#15598 = DIRECTION ( 'NONE',  ( 0.000000000000000000, 0.3090169943749481174, -0.9510565162951533091 ) ) ;
#15599 = DIRECTION ( 'NONE',  ( -1.000000000000000000, 0.000000000000000000, 0.000000000000000000 ) ) ;
#15600 = ORIENTED_EDGE ( 'NONE', *, *, #14959, .T. ) ;
#15601 = PLANE ( 'NONE',  #528 ) ;
#15602 = EDGE_LOOP ( 'NONE', ( #8456, #5383, #10385, #1058 ) ) ;
#15603 = CARTESIAN_POINT ( 'NONE',  ( 0.000000000000000000, -27.72801475327285559, 5.086963483077107995 ) ) ;
#15604 = DIRECTION ( 'NONE',  ( 0.000000000000000000, 0.000000000000000000, -1.000000000000000000 ) ) ;
#15605 = ORIENTED_EDGE ( 'NONE', *, *, #18432, .F. ) ;
#15606 = ORIENTED_EDGE ( 'NONE', *, *, #3101, .F. ) ;
#15607 = ADVANCED_FACE ( 'NONE', ( #4966 ), #12211, .T. ) ;
#15608 = CYLINDRICAL_SURFACE ( 'NONE', #1415, 24.00000000002399503 ) ;
#15609 = AXIS2_PLACEMENT_3D ( 'NONE', #11784, #11873, #7208 ) ;
#15610 = ORIENTED_EDGE ( 'NONE', *, *, #18060, .F. ) ;
#15611 = DIRECTION ( 'NONE',  ( -1.000000000000000000, -0.000000000000000000, 0.000000000000000000 ) ) ;
#15612 = CIRCLE ( 'NONE', #7677, 63.00000000006298961 ) ;
#15613 = DIRECTION ( 'NONE',  ( 1.000000000000000000, 0.000000000000000000, 0.000000000000000000 ) ) ;
#15614 = CLOSED_SHELL ( 'NONE', ( #6364, #1535, #3673, #12374, #8718, #140, #3549, #18787, #5838, #14183, #9043, #2970, #10882, #17122, #7368, #7695, #8942, #16718, #11632, #7376, #17299, #15526, #2965, #6279, #11212, #3909, #5273, #2069, #18323, #2027, #5860, #4976, #6716, #10321, #2250, #9605, #16198, #3778, #18494, #11700, #13887, #1563, #8756, #8523, #15980, #14349, #17861, #5384, #9529, #3522, #6192, #7029, #9532, #8218, #18613, #9697, #14258, #12141, #3552, #9850, #46, #3317, #14261, #2368, #10016, #14017, #6930, #1357, #228, #3760, #2689, #18547, #10020, #1080, #8785, #16283, #8003, #1434, #11975, #6336, #14597, #5473, #11758, #10855, #7312, #14507, #12514, #3622, #13144, #3781, #5220, #14105, #7968 ) ) ;
#15615 = ORIENTED_EDGE ( 'NONE', *, *, #4668, .T. ) ;
#15616 = CIRCLE ( 'NONE', #1333, 63.00000000006298961 ) ;
#15617 = ORIENTED_EDGE ( 'NONE', *, *, #7944, .F. ) ;
#15618 = LINE ( 'NONE', #5036, #7501 ) ;
#15619 = LINE ( 'NONE', #7127, #18210 ) ;
#15620 = DIRECTION ( 'NONE',  ( 0.000000000000000000, -0.8090169943749531134, 0.5877852522924654766 ) ) ;
#15621 = CARTESIAN_POINT ( 'NONE',  ( 10.00000000000000000, 0.000000000000000000, 0.000000000000000000 ) ) ;
#15622 = EDGE_CURVE ( 'NONE', #15321, #3828, #1928, .T. ) ;
#15623 = EDGE_CURVE ( 'NONE', #15108, #12463, #13634, .T. ) ;
#15624 = CYLINDRICAL_SURFACE ( 'NONE', #10581, 24.00000000002400213 ) ;
#15625 = DIRECTION ( 'NONE',  ( 1.000000000000000000, -0.000000000000000000, -0.000000000000000000 ) ) ;
#15626 = DIRECTION ( 'NONE',  ( -1.000000000000000000, 0.000000000000000000, -0.000000000000000000 ) ) ;
#15627 = ORIENTED_EDGE ( 'NONE', *, *, #1875, .F. ) ;
#15628 = CARTESIAN_POINT ( 'NONE',  ( -0.6810597143197697489, -4.461075778259609770, -3.598441714920717516 ) ) ;
#15629 = DIRECTION ( 'NONE',  ( 0.000000000000000000, -0.4539904997395540764, 0.8910065241883640130 ) ) ;
#15630 = PRODUCT_DEFINITION ( 'UNKNOWN', '', #18710, #7481 ) ;
#15631 = DIRECTION ( 'NONE',  ( 1.000000000000000000, 0.000000000000000000, 0.000000000000000000 ) ) ;
#15632 = CARTESIAN_POINT ( 'NONE',  ( -26.29305231718584324, -34.99999999999999289, 19.10302069950530779 ) ) ;
#15633 =( GEOMETRIC_REPRESENTATION_CONTEXT ( 3 ) GLOBAL_UNCERTAINTY_ASSIGNED_CONTEXT ( ( #17959 ) ) GLOBAL_UNIT_ASSIGNED_CONTEXT ( ( #11562, #4504, #10314 ) ) REPRESENTATION_CONTEXT ( 'NONE', 'WORKASPACE' ) );
#15634 = ORIENTED_EDGE ( 'NONE', *, *, #12013, .T. ) ;
#15635 = VERTEX_POINT ( 'NONE', #16313 ) ;
#15636 = EDGE_CURVE ( 'NONE', #1864, #6177, #6634, .T. ) ;
#15637 = ORIENTED_EDGE ( 'NONE', *, *, #5954, .T. ) ;
#15638 = DIRECTION ( 'NONE',  ( -0.000000000000000000, 1.000000000000000000, -0.000000000000000000 ) ) ;
#15639 = CARTESIAN_POINT ( 'NONE',  ( 2.059999999999998721, 0.000000000000000000, -0.3080913168122742518 ) ) ;
#15640 = SURFACE_SIDE_STYLE ('',( #9833 ) ) ;
#15641 = CARTESIAN_POINT ( 'NONE',  ( 4.000000000000000888, 1.563622288139206118, -0.2253451193528334950 ) ) ;
#15642 = ADVANCED_FACE ( 'NONE', ( #8966 ), #1838, .F. ) ;
#15643 = ADVANCED_FACE ( 'NONE', ( #3273 ), #3088, .T. ) ;
#15644 = DIRECTION ( 'NONE',  ( 0.000000000000000000, -1.000000000000000000, 0.000000000000000000 ) ) ;
#15645 = CARTESIAN_POINT ( 'NONE',  ( 2.500000000000000000, 0.000000000000000000, 0.000000000000000000 ) ) ;
#15646 = DIRECTION ( 'NONE',  ( -1.000000000000000000, 0.000000000000000000, -0.000000000000000000 ) ) ;
#15647 = EDGE_LOOP ( 'NONE', ( #16730, #1982, #4187, #12533 ) ) ;
#15648 = CARTESIAN_POINT ( 'NONE',  ( -4.000000000000000000, 0.1981133338132459731, 2.096406544454392723E-17 ) ) ;
#15649 = VERTEX_POINT ( 'NONE', #1642 ) ;
#15650 = EDGE_CURVE ( 'NONE', #5152, #7515, #6212, .T. ) ;
#15651 = CARTESIAN_POINT ( 'NONE',  ( 0.000000000000000000, -27.94286728106395756, 15.73043801031622912 ) ) ;
#15652 = FACE_OUTER_BOUND ( 'NONE', #11614, .T. ) ;
#15653 = VERTEX_POINT ( 'NONE', #6123 ) ;
#15654 = EDGE_CURVE ( 'NONE', #18475, #6727, #5729, .T. ) ;
#15655 = CARTESIAN_POINT ( 'NONE',  ( 3.499999999999999556, -27.60846790388774608, -2.000000000000000000 ) ) ;
#15656 = DIRECTION ( 'NONE',  ( 1.000000000000000000, 6.123233995736766036E-17, -6.123233995736764803E-17 ) ) ;
#15657 = LINE ( 'NONE', #6996, #8853 ) ;
#15658 = ORIENTED_EDGE ( 'NONE', *, *, #14475, .T. ) ;
#15659 = ADVANCED_FACE ( 'NONE', ( #6028 ), #7553, .T. ) ;
#15660 = PRESENTATION_LAYER_ASSIGNMENT (  '', '', ( #15961 ) ) ;
#15661 = AXIS2_PLACEMENT_3D ( 'NONE', #18576, #14193, #17066 ) ;
#15662 = LINE ( 'NONE', #11372, #4434 ) ;
#15663 = DIRECTION ( 'NONE',  ( 0.000000000000000000, 0.000000000000000000, 1.000000000000000000 ) ) ;
#15664 = DIRECTION ( 'NONE',  ( 0.000000000000000000, -6.938893903900289557E-15, 1.000000000000000000 ) ) ;
#15665 = LINE ( 'NONE', #4148, #8820 ) ;
#15666 = LINE ( 'NONE', #14245, #14551 ) ;
#15667 = EDGE_LOOP ( 'NONE', ( #8415, #13298, #3187, #16888 ) ) ;
#15668 = VECTOR ( 'NONE', #9001, 1000.000000000000000 ) ;
#15669 = CARTESIAN_POINT ( 'NONE',  ( 10.00000000000000000, -1.017308535512791767, 56.37237871411032586 ) ) ;
#15670 = DIRECTION ( 'NONE',  ( -1.000000000000000000, -0.000000000000000000, 0.000000000000000000 ) ) ;
#15671 = DIRECTION ( 'NONE',  ( -0.000000000000000000, 1.000000000000000000, -0.000000000000000000 ) ) ;
#15672 = ORIENTED_EDGE ( 'NONE', *, *, #3966, .F. ) ;
#15673 = AXIS2_PLACEMENT_3D ( 'NONE', #9401, #271, #10816 ) ;
#15674 = VERTEX_POINT ( 'NONE', #13375 ) ;
#15675 = AXIS2_PLACEMENT_3D ( 'NONE', #6603, #16794, #17938 ) ;
#15676 = ADVANCED_FACE ( 'NONE', ( #11931 ), #12016, .F. ) ;
#15677 = FACE_OUTER_BOUND ( 'NONE', #1716, .T. ) ;
#15678 = EDGE_LOOP ( 'NONE', ( #4176, #9171, #10207, #7637 ) ) ;
#15679 = DIRECTION ( 'NONE',  ( 0.000000000000000000, 0.000000000000000000, 1.000000000000000000 ) ) ;
#15680 = AXIS2_PLACEMENT_3D ( 'NONE', #10167, #5966, #17596 ) ;
#15681 = CARTESIAN_POINT ( 'NONE',  ( 10.00000000000000000, 0.000000000000000000, 0.000000000000000000 ) ) ;
#15682 = VECTOR ( 'NONE', #11497, 1000.000000000000000 ) ;
#15684 = CIRCLE ( 'NONE', #10219, 4.000000000000000000 ) ;
#15683 = CARTESIAN_POINT ( 'NONE',  ( 10.00000000000000000, 55.74967257055894265, -7.478235706488370660 ) ) ;
#15685 = ORIENTED_EDGE ( 'NONE', *, *, #1330, .T. ) ;
#15686 = CARTESIAN_POINT ( 'NONE',  ( -10.00000000000000000, -42.79754323328189969, -11.25576474687263229 ) ) ;
#15687 = VERTEX_POINT ( 'NONE', #14027 ) ;
#15688 = CARTESIAN_POINT ( 'NONE',  ( -56.50000000009000445, -38.00000000000000000, 3.817814120399276590E-13 ) ) ;
#15689 = DIRECTION ( 'NONE',  ( 0.000000000000000000, 0.000000000000000000, 1.000000000000000000 ) ) ;
#15690 = CARTESIAN_POINT ( 'NONE',  ( 10.00000000000000000, -55.33199130079790962, 10.11537145609357502 ) ) ;
#15691 = ORIENTED_EDGE ( 'NONE', *, *, #12782, .F. ) ;
#15692 = CARTESIAN_POINT ( 'NONE',  ( 10.00000000000000000, 25.42247726998014912, 12.18267823974760411 ) ) ;
#15693 = ORIENTED_EDGE ( 'NONE', *, *, #14365, .F. ) ;
#15694 = DIRECTION ( 'NONE',  ( 1.000000000000000000, -0.000000000000000000, -0.000000000000000000 ) ) ;
#15695 = DIRECTION ( 'NONE',  ( -1.000000000000000000, -0.000000000000000000, -0.000000000000000000 ) ) ;
#15696 = CIRCLE ( 'NONE', #3523, 12.00000000001200462 ) ;
#15697 = ORIENTED_EDGE ( 'NONE', *, *, #14019, .T. ) ;
#15698 = VERTEX_POINT ( 'NONE', #11054 ) ;
#15699 = CIRCLE ( 'NONE', #185, 4.000000000000000000 ) ;
#15700 = EDGE_CURVE ( 'NONE', #9007, #15320, #15159, .T. ) ;
#15701 = DIRECTION ( 'NONE',  ( -1.000000000000000000, 0.000000000000000000, -0.000000000000000000 ) ) ;
#15702 = SURFACE_SIDE_STYLE ('',( #7114 ) ) ;
#15703 = ORIENTED_EDGE ( 'NONE', *, *, #15982, .F. ) ;
#15704 = DIRECTION ( 'NONE',  ( 0.1305261922200516844, 0.9914448613738103822, -0.000000000000000000 ) ) ;
#15705 = CARTESIAN_POINT ( 'NONE',  ( 1.836970198721030062E-14, 10.00000000000000000, 150.0000000000000284 ) ) ;
#15706 = VECTOR ( 'NONE', #15202, 1000.000000000000000 ) ;
#15707 = CIRCLE ( 'NONE', #7477, 2.649999999999999467 ) ;
#15708 = APPLICATION_CONTEXT ( 'automotive_design' ) ;
#15709 = CIRCLE ( 'NONE', #11127, 12.00000000001200462 ) ;
#15710 =( GEOMETRIC_REPRESENTATION_CONTEXT ( 3 ) GLOBAL_UNCERTAINTY_ASSIGNED_CONTEXT ( ( #15486 ) ) GLOBAL_UNIT_ASSIGNED_CONTEXT ( ( #4476, #12962, #13060 ) ) REPRESENTATION_CONTEXT ( 'NONE', 'WORKASPACE' ) );
#15711 = ADVANCED_FACE ( 'NONE', ( #791 ), #6950, .F. ) ;
#15712 = VERTEX_POINT ( 'NONE', #18304 ) ;
#15713 = VECTOR ( 'NONE', #18596, 1000.000000000000000 ) ;
#15714 = AXIS2_PLACEMENT_3D ( 'NONE', #18388, #6494, #5347 ) ;
#15715 = ORIENTED_EDGE ( 'NONE', *, *, #4003, .F. ) ;
#15716 = FACE_OUTER_BOUND ( 'NONE', #10406, .T. ) ;
#15717 = AXIS2_PLACEMENT_3D ( 'NONE', #18338, #7285, #1481 ) ;
#15718 = CARTESIAN_POINT ( 'NONE',  ( -3.510273485745307287, -2.827716139362669967, -3.610536846335890004 ) ) ;
#15719 = DIRECTION ( 'NONE',  ( 0.000000000000000000, -0.9510565162951500895, -0.3090169943749581649 ) ) ;
#15720 = CARTESIAN_POINT ( 'NONE',  ( 0.000000000000000000, 0.000000000000000000, 0.000000000000000000 ) ) ;
#15721 = EDGE_CURVE ( 'NONE', #11633, #6555, #11522, .T. ) ;
#15722 = CARTESIAN_POINT ( 'NONE',  ( 11.24999999999999645, 0.000000000000000000, 25.10000000000000142 ) ) ;
#15723 = DIRECTION ( 'NONE',  ( -0.5000000000000051070, 1.060575238724903217E-16, -0.8660254037844355990 ) ) ;
#15724 = CARTESIAN_POINT ( 'NONE',  ( 10.04305231718579705, -26.50000000000000000, 30.90933677959249337 ) ) ;
#15725 = ORIENTED_EDGE ( 'NONE', *, *, #11451, .F. ) ;
#15726 = CARTESIAN_POINT ( 'NONE',  ( 10.04305231718579705, -30.00000000000000000, 30.90933677959249337 ) ) ;
#15727 = CYLINDRICAL_SURFACE ( 'NONE', #12988, 10.00000000000000888 ) ;
#15728 = DIRECTION ( 'NONE',  ( 1.000000000000000000, 0.000000000000000000, 0.000000000000000000 ) ) ;
#15729 = CARTESIAN_POINT ( 'NONE',  ( -90.00000000009001155, -88.00000000000000000, -27.50000000000000000 ) ) ;
#15730 = AXIS2_PLACEMENT_3D ( 'NONE', #4736, #12176, #10731 ) ;
#15731 = MECHANICAL_DESIGN_GEOMETRIC_PRESENTATION_REPRESENTATION (  '', ( #10838 ), #6897 ) ;
#15732 = CIRCLE ( 'NONE', #10243, 4.799999999999999822 ) ;
#15733 = ORIENTED_EDGE ( 'NONE', *, *, #177, .F. ) ;
#15734 = AXIS2_PLACEMENT_3D ( 'NONE', #16110, #2973, #6453 ) ;
#15735 = ORIENTED_EDGE ( 'NONE', *, *, #12370, .T. ) ;
#15736 = DIRECTION ( 'NONE',  ( -0.000000000000000000, 1.000000000000000000, -0.000000000000000000 ) ) ;
#15737 = CYLINDRICAL_SURFACE ( 'NONE', #9141, 26.24900000002624978 ) ;
#15738 = AXIS2_PLACEMENT_3D ( 'NONE', #6370, #10451, #12178 ) ;
#15739 = EDGE_LOOP ( 'NONE', ( #17946, #9544, #8973, #8421 ) ) ;
#15740 = SURFACE_STYLE_FILL_AREA ( #4119 ) ;
#15741 = DIRECTION ( 'NONE',  ( -1.000000000000000000, 0.000000000000000000, -0.000000000000000000 ) ) ;
#15742 = VECTOR ( 'NONE', #7027, 1000.000000000000000 ) ;
#15743 = DIRECTION ( 'NONE',  ( 0.000000000000000000, -0.9876883405951394357, 0.1564344650402205994 ) ) ;
#15744 = FACE_OUTER_BOUND ( 'NONE', #4184, .T. ) ;
#15745 = AXIS2_PLACEMENT_3D ( 'NONE', #18241, #18528, #5091 ) ;
#15746 = CARTESIAN_POINT ( 'NONE',  ( 10.00000000000000000, -27.72801475327278453, -5.086963483077506787 ) ) ;
#15747 = ORIENTED_EDGE ( 'NONE', *, *, #3498, .F. ) ;
#15748 = LINE ( 'NONE', #17178, #3945 ) ;
#15749 = ORIENTED_EDGE ( 'NONE', *, *, #11187, .T. ) ;
#15750 = PRODUCT ( 'spur gear_iso_ISO - Spur gear 3M 20T 20PA 10FW ---S20A75H50L10.0S1', 'spur gear_iso_ISO - Spur gear 3M 20T 20PA 10FW ---S20A75H50L10.0S1', '', ( #1283 ) ) ;
#15751 = DIRECTION ( 'NONE',  ( -1.000000000000000000, 0.000000000000000000, 0.000000000000000000 ) ) ;
#15752 = CARTESIAN_POINT ( 'NONE',  ( -10.00000000000000000, 0.000000000000000000, 0.000000000000000000 ) ) ;
#15753 = ORIENTED_EDGE ( 'NONE', *, *, #2374, .F. ) ;
#15754 = APPLICATION_PROTOCOL_DEFINITION ( 'draft international standard', 'automotive_design', 1998, #2206 ) ;
#15755 = DIRECTION ( 'NONE',  ( 0.000000000000000000, 0.000000000000000000, 1.000000000000000000 ) ) ;
#15756 = VERTEX_POINT ( 'NONE', #16881 ) ;
#15757 = EDGE_CURVE ( 'NONE', #13284, #79, #13346, .T. ) ;
#15758 = EDGE_CURVE ( 'NONE', #7847, #16606, #1484, .T. ) ;
#15759 = CIRCLE ( 'NONE', #6630, 2.649999999999999467 ) ;
#15760 = EDGE_CURVE ( 'NONE', #12166, #7753, #18391, .T. ) ;
#15761 = AXIS2_PLACEMENT_3D ( 'NONE', #13003, #13099, #8432 ) ;
#15762 = VECTOR ( 'NONE', #31, 1000.000000000000000 ) ;
#15763 = DIRECTION ( 'NONE',  ( -1.000000000000000000, 0.000000000000000000, -0.000000000000000000 ) ) ;
#15764 = EDGE_CURVE ( 'NONE', #5108, #1683, #5349, .T. ) ;
#15765 = DIRECTION ( 'NONE',  ( -1.000000000000000000, 0.000000000000000000, 0.000000000000000000 ) ) ;
#15766 = CARTESIAN_POINT ( 'NONE',  ( -10.00000000000000000, -26.45033635316118747, 36.40576474687271258 ) ) ;
#15767 = CARTESIAN_POINT ( 'NONE',  ( 2.500000000000000000, 1.178949249685212974, -2.042000000000001148 ) ) ;
#15768 = ADVANCED_FACE ( 'NONE', ( #15179 ), #2121, .T. ) ;
#15769 = AXIS2_PLACEMENT_3D ( 'NONE', #16625, #3865, #3590 ) ;
#15770 = DIRECTION ( 'NONE',  ( 1.000000000000000000, -0.000000000000000000, 0.000000000000000000 ) ) ;
#15771 = ORIENTED_EDGE ( 'NONE', *, *, #13504, .F. ) ;
#15772 = AXIS2_PLACEMENT_3D ( 'NONE', #10480, #16299, #7719 ) ;
#15773 = CARTESIAN_POINT ( 'NONE',  ( 0.000000000000000000, 24.97244012287581327, -57.83923611457294101 ) ) ;
#15774 = EDGE_CURVE ( 'NONE', #18250, #5010, #5738, .T. ) ;
#15775 = CARTESIAN_POINT ( 'NONE',  ( 10.00000000000000000, 49.76630880786347433, -26.49895292617950560 ) ) ;
#15776 = CARTESIAN_POINT ( 'NONE',  ( 10.00000000000000000, -27.72801475327285559, 5.086963483077107995 ) ) ;
#15777 = ORIENTED_EDGE ( 'NONE', *, *, #8767, .T. ) ;
#15778 = ORIENTED_EDGE ( 'NONE', *, *, #5553, .T. ) ;
#15779 = DIRECTION ( 'NONE',  ( 0.000000000000000000, 0.000000000000000000, 1.000000000000000000 ) ) ;
#15780 = ORIENTED_EDGE ( 'NONE', *, *, #5274, .F. ) ;
#15781 = CARTESIAN_POINT ( 'NONE',  ( 45.00000000000000000, 10.00000000000000000, -2.650000000000511946 ) ) ;
#15782 = EDGE_CURVE ( 'NONE', #15213, #10765, #9069, .T. ) ;
#15783 = AXIS2_PLACEMENT_3D ( 'NONE', #8231, #14034, #2216 ) ;
#15784 = CIRCLE ( 'NONE', #7562, 2.649999999999999467 ) ;
#15785 = LINE ( 'NONE', #17316, #2294 ) ;
#15786 = CIRCLE ( 'NONE', #14870, 2.649999999999999467 ) ;
#15787 =( GEOMETRIC_REPRESENTATION_CONTEXT ( 3 ) GLOBAL_UNCERTAINTY_ASSIGNED_CONTEXT ( ( #12617 ) ) GLOBAL_UNIT_ASSIGNED_CONTEXT ( ( #4491, #4581, #16290 ) ) REPRESENTATION_CONTEXT ( 'NONE', 'WORKASPACE' ) );
#15788 = VECTOR ( 'NONE', #3337, 1000.000000000000000 ) ;
#15789 = CARTESIAN_POINT ( 'NONE',  ( 4.999999999999999112, 61.47135697633798657, -13.79392154159068618 ) ) ;
#15790 = EDGE_CURVE ( 'NONE', #3687, #2800, #1177, .T. ) ;
#15791 = ORIENTED_EDGE ( 'NONE', *, *, #15569, .F. ) ;
#15792 = CARTESIAN_POINT ( 'NONE',  ( 10.00000000000000000, -16.45250512421895550, 53.92768374110886498 ) ) ;
#15793 = ORIENTED_EDGE ( 'NONE', *, *, #6922, .T. ) ;
#15794 = DIRECTION ( 'NONE',  ( 0.000000000000000000, -1.000000000000000000, 0.000000000000000000 ) ) ;
#15795 = EDGE_LOOP ( 'NONE', ( #9024, #17500, #7267, #17817 ) ) ;
#15796 = DIRECTION ( 'NONE',  ( 0.000000000000000000, 0.000000000000000000, 1.000000000000000000 ) ) ;
#15797 = ORIENTED_EDGE ( 'NONE', *, *, #16542, .T. ) ;
#15798 = CYLINDRICAL_SURFACE ( 'NONE', #17913, 24.00000000002399858 ) ;
#15799 = CARTESIAN_POINT ( 'NONE',  ( 0.6937372685066666156, -4.453844082567737672, -3.610536846335894445 ) ) ;
#15800 = CIRCLE ( 'NONE', #13065, 24.00000000002400213 ) ;
#15801 = ORIENTED_EDGE ( 'NONE', *, *, #15884, .T. ) ;
#15802 = ORIENTED_EDGE ( 'NONE', *, *, #14758, .F. ) ;
#15803 = CARTESIAN_POINT ( 'NONE',  ( 0.000000000000000000, -30.00000000000000000, 0.000000000000000000 ) ) ;
#15804 = SURFACE_STYLE_USAGE ( .BOTH. , #12290 ) ;
#15805 = ORIENTED_EDGE ( 'NONE', *, *, #5887, .F. ) ;
#15806 = DIRECTION ( 'NONE',  ( -0.000000000000000000, -1.000000000000000000, -0.000000000000000000 ) ) ;
#15807 = DIRECTION ( 'NONE',  ( 1.000000000000000000, 0.000000000000000000, 0.000000000000000000 ) ) ;
#15808 = CYLINDRICAL_SURFACE ( 'NONE', #14648, 20.00000000000000000 ) ;
#15809 = AXIS2_PLACEMENT_3D ( 'NONE', #17522, #7236, #10286 ) ;
#15810 = EDGE_CURVE ( 'NONE', #7876, #15559, #3301, .T. ) ;
#15811 = EDGE_LOOP ( 'NONE', ( #10274, #2160, #13859, #8651 ) ) ;
#15812 = AXIS2_PLACEMENT_3D ( 'NONE', #5294, #11099, #16922 ) ;
#15813 = MANIFOLD_SOLID_BREP ( 'M5 Clearance Hole2', #3143 ) ;
#15814 = ORIENTED_EDGE ( 'NONE', *, *, #14132, .F. ) ;
#15815 = CYLINDRICAL_SURFACE ( 'NONE', #210, 24.00000000002399858 ) ;
#15816 = CARTESIAN_POINT ( 'NONE',  ( 10.00000000000000000, 0.000000000000000000, 0.000000000000000000 ) ) ;
#15817 = DIRECTION ( 'NONE',  ( -0.000000000000000000, -0.000000000000000000, 1.000000000000000000 ) ) ;
#15818 = DIRECTION ( 'NONE',  ( 0.000000000000000000, -6.982962677686266711E-15, 1.000000000000000000 ) ) ;
#15819 = CARTESIAN_POINT ( 'NONE',  ( 0.000000000000000000, -2.357898499370431722, 2.818925648462311528E-15 ) ) ;
#15820 = DIRECTION ( 'NONE',  ( 0.000000000000000000, 0.000000000000000000, 1.000000000000000000 ) ) ;
#15821 = CARTESIAN_POINT ( 'NONE',  ( -79.64793068852927149, -34.99999999999999289, 31.86039329588764701 ) ) ;
#15822 = ORIENTED_EDGE ( 'NONE', *, *, #295, .F. ) ;
#15823 = DIRECTION ( 'NONE',  ( 0.000000000000000000, 1.000000000000000000, 0.000000000000000000 ) ) ;
#15824 = CARTESIAN_POINT ( 'NONE',  ( 13.90576474687263264, 10.00000000000000000, -40.14754323328190111 ) ) ;
#15825 = VERTEX_POINT ( 'NONE', #2299 ) ;
#15826 = CYLINDRICAL_SURFACE ( 'NONE', #12111, 27.00000000000000355 ) ;
#15827 = AXIS2_PLACEMENT_3D ( 'NONE', #1299, #15671, #12913 ) ;
#15828 = CARTESIAN_POINT ( 'NONE',  ( 4.999999999999997335, 0.000000000000000000, 0.000000000000000000 ) ) ;
#15829 = AXIS2_PLACEMENT_3D ( 'NONE', #9185, #10987, #7751 ) ;
#15830 = EDGE_CURVE ( 'NONE', #16445, #18269, #572, .T. ) ;
#15831 = ORIENTED_EDGE ( 'NONE', *, *, #6322, .F. ) ;
#15832 = ADVANCED_FACE ( 'NONE', ( #17446 ), #12888, .T. ) ;
#15833 = ORIENTED_EDGE ( 'NONE', *, *, #7119, .T. ) ;
#15834 = DIRECTION ( 'NONE',  ( 0.000000000000000000, -1.000000000000000000, 0.000000000000000000 ) ) ;
#15835 = ORIENTED_EDGE ( 'NONE', *, *, #3137, .F. ) ;
#15836 = DIRECTION ( 'NONE',  ( 0.000000000000000000, 0.000000000000000000, 1.000000000000000000 ) ) ;
#15837 = CARTESIAN_POINT ( 'NONE',  ( 0.000000000000000000, 5.051668046482832750E-16, -4.000000000000000000 ) ) ;
#15838 = CARTESIAN_POINT ( 'NONE',  ( 0.000000000000000000, 0.000000000000000000, 0.000000000000000000 ) ) ;
#15839 = CARTESIAN_POINT ( 'NONE',  ( 10.00000000000000000, -24.97244012287543313, 57.83923611457311154 ) ) ;
#15840 = DIRECTION ( 'NONE',  ( 0.000000000000000000, 0.000000000000000000, 1.000000000000000000 ) ) ;
#15841 = ORIENTED_EDGE ( 'NONE', *, *, #12721, .F. ) ;
#15842 = DIRECTION ( 'NONE',  ( 0.000000000000000000, 0.000000000000000000, 1.000000000000000000 ) ) ;
#15843 = ORIENTED_EDGE ( 'NONE', *, *, #13504, .T. ) ;
#15844 = FILL_AREA_STYLE ('',( #18695 ) ) ;
#15845 = FACE_OUTER_BOUND ( 'NONE', #8285, .T. ) ;
#15846 = ORIENTED_EDGE ( 'NONE', *, *, #18325, .F. ) ;
#15847 = MANIFOLD_SOLID_BREP ( 'Keyway', #15614 ) ;
#15848 = PRODUCT_CONTEXT ( 'NONE', #10116, 'mechanical' ) ;
#15849 = CARTESIAN_POINT ( 'NONE',  ( 0.000000000000000000, -30.00000000000000000, 0.000000000000000000 ) ) ;
#15850 = ORIENTED_EDGE ( 'NONE', *, *, #3376, .F. ) ;
#15851 =( REPRESENTATION_RELATIONSHIP ('NONE','NONE', #11014, #2517 ) REPRESENTATION_RELATIONSHIP_WITH_TRANSFORMATION ( #14578 )SHAPE_REPRESENTATION_RELATIONSHIP( ) );
#15852 = PRESENTATION_LAYER_ASSIGNMENT (  '', '', ( #2773 ) ) ;
#15853 = ORIENTED_EDGE ( 'NONE', *, *, #18307, .F. ) ;
#15854 = CARTESIAN_POINT ( 'NONE',  ( 10.00000000000000000, 53.29895248911700634, -18.38754094778185788 ) ) ;
#15855 = CARTESIAN_POINT ( 'NONE',  ( 10.00000000000000000, 33.95787273855245303, 45.00825343885033192 ) ) ;
#15856 = CARTESIAN_POINT ( 'NONE',  ( 10.00000000000000000, -7.478235706488566059, -55.74967257055892134 ) ) ;
#15857 = CARTESIAN_POINT ( 'NONE',  ( 10.00000000000000000, -16.45250512421816680, -53.92768374110909235 ) ) ;
#15858 = CARTESIAN_POINT ( 'NONE',  ( -90.00000000009001155, -10.00000000000001776, -1.301042606982605912E-15 ) ) ;
#15859 = ORIENTED_EDGE ( 'NONE', *, *, #8193, .F. ) ;
#15860 = EDGE_CURVE ( 'NONE', #9916, #7866, #14315, .T. ) ;
#15861 = CIRCLE ( 'NONE', #9463, 63.00000000006298961 ) ;
#15862 = EDGE_CURVE ( 'NONE', #14912, #9858, #1271, .T. ) ;
#15863 = CYLINDRICAL_SURFACE ( 'NONE', #16924, 63.00000000006298961 ) ;
#15864 = DIRECTION ( 'NONE',  ( -1.000000000000000000, 0.000000000000000000, -0.000000000000000000 ) ) ;
#15865 = DIRECTION ( 'NONE',  ( 1.000000000000000000, 0.000000000000000000, 0.000000000000000000 ) ) ;
#15866 = EDGE_LOOP ( 'NONE', ( #5199, #14515, #4748, #3279, #17482 ) ) ;
#15867 = ORIENTED_EDGE ( 'NONE', *, *, #6488, .T. ) ;
#15868 = DIRECTION ( 'NONE',  ( 0.000000000000000000, 0.5877852522924685852, 0.8090169943749506709 ) ) ;
#15869 =( NAMED_UNIT ( * ) PLANE_ANGLE_UNIT ( ) SI_UNIT ( $, .RADIAN. ) );
#15870 = VERTEX_POINT ( 'NONE', #1450 ) ;
#15871 = EDGE_CURVE ( 'NONE', #15970, #11257, #9375, .T. ) ;
#15872 = DIRECTION ( 'NONE',  ( -0.000000000000000000, -1.000000000000000000, -0.000000000000000000 ) ) ;
#15873 = EDGE_CURVE ( 'NONE', #5391, #4075, #8473, .T. ) ;
#15874 = DIRECTION ( 'NONE',  ( 0.000000000000000000, 1.000000000000000000, 0.000000000000000000 ) ) ;
#15875 = EDGE_LOOP ( 'NONE', ( #6932, #3237, #9994, #6484 ) ) ;
#15876 = DIRECTION ( 'NONE',  ( -1.000000000000000000, 0.000000000000000000, 0.000000000000000000 ) ) ;
#15877 = VECTOR ( 'NONE', #18658, 1000.000000000000000 ) ;
#15878 = VERTEX_POINT ( 'NONE', #16014 ) ;
#15879 = CARTESIAN_POINT ( 'NONE',  ( -90.00000000009001155, -38.00000000000000000, -1.301042606982603940E-15 ) ) ;
#15880 = VERTEX_POINT ( 'NONE', #28 ) ;
#15881 = CARTESIAN_POINT ( 'NONE',  ( -31.74999999999995737, 0.000000000000000000, 0.000000000000000000 ) ) ;
#15883 = ORIENTED_EDGE ( 'NONE', *, *, #6461, .F. ) ;
#15882 = EDGE_CURVE ( 'NONE', #17177, #16873, #18686, .T. ) ;
#15884 = EDGE_CURVE ( 'NONE', #6907, #15225, #8776, .T. ) ;
#15885 = FACE_OUTER_BOUND ( 'NONE', #18769, .T. ) ;
#15886 = DIRECTION ( 'NONE',  ( 0.000000000000000000, -6.938893903900288768E-15, 1.000000000000000000 ) ) ;
#15887 = ORIENTED_EDGE ( 'NONE', *, *, #2849, .F. ) ;
#15888 = ORIENTED_EDGE ( 'NONE', *, *, #6450, .F. ) ;
#15889 = DIRECTION ( 'NONE',  ( -1.000000000000000000, 0.000000000000000000, -0.000000000000000000 ) ) ;
#15890 = EDGE_CURVE ( 'NONE', #9389, #13064, #9991, .T. ) ;
#15891 = ORIENTED_EDGE ( 'NONE', *, *, #5295, .F. ) ;
#15892 = CARTESIAN_POINT ( 'NONE',  ( 0.000000000000000000, 56.23315539212690339, 1.335003989221828835 ) ) ;
#15893 = EDGE_CURVE ( 'NONE', #10272, #10656, #1772, .T. ) ;
#15894 = AXIS2_PLACEMENT_3D ( 'NONE', #1159, #9619, #8205 ) ;
#15895 = CARTESIAN_POINT ( 'NONE',  ( 23.48826165280196321, 11.24999999999999467, 0.7426739052322660628 ) ) ;
#15896 = ORIENTED_EDGE ( 'NONE', *, *, #15979, .F. ) ;
#15897 = PRODUCT_DEFINITION_SHAPE ( 'NONE', 'NONE',  #18820 ) ;
#15898 = MANIFOLD_SOLID_BREP ( 'Hex', #105 ) ;
#15899 = ORIENTED_EDGE ( 'NONE', *, *, #7405, .F. ) ;
#15900 = FACE_OUTER_BOUND ( 'NONE', #6151, .T. ) ;
#15901 = CARTESIAN_POINT ( 'NONE',  ( 10.00000000000000000, 0.000000000000000000, 0.000000000000000000 ) ) ;
#15902 = DIRECTION ( 'NONE',  ( 0.000000000000000000, 0.5877852522924684742, 0.8090169943749506709 ) ) ;
#15903 = LINE ( 'NONE', #18478, #14831 ) ;
#15904 = CARTESIAN_POINT ( 'NONE',  ( 10.00000000000000000, -25.42247726998005675, -12.18267823974779240 ) ) ;
#15905 = LINE ( 'NONE', #7131, #2077 ) ;
#15907 = CIRCLE ( 'NONE', #6776, 2.649999999999999467 ) ;
#15906 = DIRECTION ( 'NONE',  ( -0.000000000000000000, 1.000000000000000000, -0.000000000000000000 ) ) ;
#15908 = CARTESIAN_POINT ( 'NONE',  ( 10.00000000000000000, -14.19907017806852245, -22.07705612348854984 ) ) ;
#15909 = ORIENTED_EDGE ( 'NONE', *, *, #1098, .F. ) ;
#15910 = AXIS2_PLACEMENT_3D ( 'NONE', #15828, #11630, #2777 ) ;
#15911 = DIRECTION ( 'NONE',  ( 0.000000000000000000, 0.000000000000000000, 1.000000000000000000 ) ) ;
#15912 = DIRECTION ( 'NONE',  ( 0.000000000000000000, 0.000000000000000000, 1.000000000000000000 ) ) ;
#15913 = VERTEX_POINT ( 'NONE', #17537 ) ;
#15914 = CARTESIAN_POINT ( 'NONE',  ( 0.000000000000000000, 0.000000000000000000, -1.000000000000000000 ) ) ;
#15915 = CYLINDRICAL_SURFACE ( 'NONE', #11030, 63.00000000006298961 ) ;
#15916 = ADVANCED_FACE ( 'NONE', ( #16397 ), #17270, .T. ) ;
#15917 = ORIENTED_EDGE ( 'NONE', *, *, #14691, .T. ) ;
#15918 = CIRCLE ( 'NONE', #8903, 24.00000000002399503 ) ;
#15919 = CIRCLE ( 'NONE', #10138, 10.00000000000000888 ) ;
#15920 = ORIENTED_EDGE ( 'NONE', *, *, #8988, .F. ) ;
#15921 = LINE ( 'NONE', #11635, #15105 ) ;
#15922 = DIRECTION ( 'NONE',  ( 0.000000000000000000, 0.9876883405951382144, -0.1564344650402274828 ) ) ;
#15923 = EDGE_LOOP ( 'NONE', ( #7224, #8627 ) ) ;
#15924 = FACE_BOUND ( 'NONE', #16497, .T. ) ;
#15925 = CARTESIAN_POINT ( 'NONE',  ( 6.080745460913608902, 0.5192545390863916310, 0.000000000000000000 ) ) ;
#15926 = DIRECTION ( 'NONE',  ( 0.000000000000000000, 0.000000000000000000, -1.000000000000000000 ) ) ;
#15927 = CARTESIAN_POINT ( 'NONE',  ( -36.40576474687271258, 0.000000000000000000, -26.45033635316118747 ) ) ;
#15928 = VERTEX_POINT ( 'NONE', #7708 ) ;
#15929 = CYLINDRICAL_SURFACE ( 'NONE', #3328, 56.24900000005625600 ) ;
#15930 = VERTEX_POINT ( 'NONE', #3066 ) ;
#15931 = VECTOR ( 'NONE', #8618, 1000.000000000000114 ) ;
#15932 = DIRECTION ( 'NONE',  ( -1.000000000000000000, 0.000000000000000000, 0.000000000000000000 ) ) ;
#15933 = FACE_OUTER_BOUND ( 'NONE', #5191, .T. ) ;
#15934 = VERTEX_POINT ( 'NONE', #11826 ) ;
#15935 = MANIFOLD_SOLID_BREP ( 'Cut-Extrude-Thin1', #2223 ) ;
#15936 = ADVANCED_FACE ( 'NONE', ( #10386 ), #10305, .F. ) ;
#15937 = ORIENTED_EDGE ( 'NONE', *, *, #6267, .T. ) ;
#15938 = ORIENTED_EDGE ( 'NONE', *, *, #14691, .F. ) ;
#15939 = CIRCLE ( 'NONE', #7717, 25.00000000000000000 ) ;
#15940 = DIRECTION ( 'NONE',  ( -1.000000000000000000, 0.000000000000000000, 0.000000000000000000 ) ) ;
#15941 = CYLINDRICAL_SURFACE ( 'NONE', #6999, 12.00000000001200462 ) ;
#15942 = DIRECTION ( 'NONE',  ( 0.000000000000000000, 0.000000000000000000, 1.000000000000000000 ) ) ;
#15943 = EDGE_CURVE ( 'NONE', #7149, #10237, #17017, .T. ) ;
#15944 = DIRECTION ( 'NONE',  ( -1.000000000000000000, -0.000000000000000000, 0.000000000000000000 ) ) ;
#15945 = CARTESIAN_POINT ( 'NONE',  ( -11.25000000000000355, 3.429011037612589670E-15, 28.00000000000000355 ) ) ;
#15946 = EDGE_LOOP ( 'NONE', ( #9955, #893, #15586, #13410 ) ) ;
#15947 = EDGE_CURVE ( 'NONE', #10659, #3659, #16202, .T. ) ;
#15948 = CARTESIAN_POINT ( 'NONE',  ( 0.000000000000000000, 53.29895248911675765, 18.38754094778260040 ) ) ;
#15949 = DIRECTION ( 'NONE',  ( 0.1305261922200517399, -0.9914448613738104932, 0.000000000000000000 ) ) ;
#15950 = DIRECTION ( 'NONE',  ( 0.000000000000000000, 0.000000000000000000, 1.000000000000000000 ) ) ;
#15951 = VERTEX_POINT ( 'NONE', #206 ) ;
#15952 = EDGE_LOOP ( 'NONE', ( #7305, #9840, #2586, #7222 ) ) ;
#15953 =( REPRESENTATION_RELATIONSHIP ('NONE','NONE', #11014, #2517 ) REPRESENTATION_RELATIONSHIP_WITH_TRANSFORMATION ( #15542 )SHAPE_REPRESENTATION_RELATIONSHIP( ) );
#15954 = FACE_OUTER_BOUND ( 'NONE', #14636, .T. ) ;
#15955 = ORIENTED_EDGE ( 'NONE', *, *, #15541, .F. ) ;
#15956 = FACE_BOUND ( 'NONE', #14018, .T. ) ;
#15957 = ADVANCED_FACE ( 'NONE', ( #7623 ), #1907, .F. ) ;
#15958 = DIRECTION ( 'NONE',  ( 0.000000000000000000, 0.000000000000000000, 1.000000000000000000 ) ) ;
#15959 = LINE ( 'NONE', #7198, #6618 ) ;
#15960 = ORIENTED_EDGE ( 'NONE', *, *, #17636, .F. ) ;
#15961 = STYLED_ITEM ( 'NONE', ( #2817 ), #17412 ) ;
#15962 = CIRCLE ( 'NONE', #17800, 56.24900000005625600 ) ;
#15963 = ORIENTED_EDGE ( 'NONE', *, *, #17395, .F. ) ;
#15964 = FACE_BOUND ( 'NONE', #9251, .T. ) ;
#15965 = CIRCLE ( 'NONE', #3494, 63.00000000006298961 ) ;
#15966 = ORIENTED_EDGE ( 'NONE', *, *, #767, .T. ) ;
#15967 = ORIENTED_EDGE ( 'NONE', *, *, #8039, .F. ) ;
#15968 = CARTESIAN_POINT ( 'NONE',  ( 45.00000000000000000, 10.00000000000000000, -5.120903701083534543E-13 ) ) ;
#15969 = PLANE ( 'NONE',  #8891 ) ;
#15970 = VERTEX_POINT ( 'NONE', #4671 ) ;
#15971 = ORIENTED_EDGE ( 'NONE', *, *, #10295, .F. ) ;
#15972 = CARTESIAN_POINT ( 'NONE',  ( -26.29305231718584324, -30.00000000000000000, 19.10302069950530779 ) ) ;
#15973 = SURFACE_STYLE_USAGE ( .BOTH. , #13130 ) ;
#15974 = VERTEX_POINT ( 'NONE', #16484 ) ;
#15975 = CYLINDRICAL_SURFACE ( 'NONE', #5767, 20.00000000000000000 ) ;
#15976 = ADVANCED_FACE ( 'NONE', ( #14498, #13085 ), #5562, .F. ) ;
#15977 = AXIS2_PLACEMENT_3D ( 'NONE', #8351, #6536, #8060 ) ;
#15978 = VECTOR ( 'NONE', #10878, 1000.000000000000000 ) ;
#15979 = EDGE_CURVE ( 'NONE', #7704, #15432, #14957, .T. ) ;
#15980 = ADVANCED_FACE ( 'NONE', ( #9234 ), #6102, .T. ) ;
#15981 = CARTESIAN_POINT ( 'NONE',  ( -290.0000000000001705, -30.00000000000000000, 125.0000000000000000 ) ) ;
#15982 = EDGE_CURVE ( 'NONE', #5875, #18738, #15052, .T. ) ;
#15983 = ORIENTED_EDGE ( 'NONE', *, *, #10294, .T. ) ;
#15984 = ADVANCED_FACE ( 'NONE', ( #15245 ), #5041, .F. ) ;
#15985 = AXIS2_PLACEMENT_3D ( 'NONE', #2908, #2727, #11383 ) ;
#15986 = EDGE_LOOP ( 'NONE', ( #15733, #15883 ) ) ;
#15987 = CYLINDRICAL_SURFACE ( 'NONE', #5373, 12.00000000001200462 ) ;
#15988 = DIRECTION ( 'NONE',  ( -1.000000000000000000, 0.000000000000000000, -0.000000000000000000 ) ) ;
#15989 = FACE_OUTER_BOUND ( 'NONE', #10123, .T. ) ;
#15990 = CYLINDRICAL_SURFACE ( 'NONE', #841, 2.649999999999992806 ) ;
#15991 = DIRECTION ( 'NONE',  ( 0.000000000000000000, 0.000000000000000000, 1.000000000000000000 ) ) ;
#15992 = EDGE_CURVE ( 'NONE', #3056, #10759, #11038, .T. ) ;
#15993 = CARTESIAN_POINT ( 'NONE',  ( 0.000000000000000000, 27.72801475327274900, 5.086963483077687975 ) ) ;
#15994 = DIRECTION ( 'NONE',  ( 0.000000000000000000, 0.000000000000000000, 1.000000000000000000 ) ) ;
#15995 = EDGE_CURVE ( 'NONE', #9845, #14286, #4950, .T. ) ;
#15996 = AXIS2_PLACEMENT_3D ( 'NONE', #7276, #11655, #2713 ) ;
#15997 = CARTESIAN_POINT ( 'NONE',  ( -4.799999999999999822, 5.878304635907294211E-16, -1.000000000000000000 ) ) ;
#15998 = ORIENTED_EDGE ( 'NONE', *, *, #16227, .F. ) ;
#15999 = CARTESIAN_POINT ( 'NONE',  ( 10.00000000000000000, 25.38428207620331634, -6.681932690256706664 ) ) ;
#16000 = CIRCLE ( 'NONE', #9604, 2.700000000000000622 ) ;
#16001 = SURFACE_SIDE_STYLE ('',( #17254 ) ) ;
#16002 = ADVANCED_FACE ( 'NONE', ( #8097 ), #10753, .T. ) ;
#16003 = ORIENTED_EDGE ( 'NONE', *, *, #11613, .F. ) ;
#16004 = DIRECTION ( 'NONE',  ( 1.000000000000000000, 0.000000000000000000, 0.000000000000000000 ) ) ;
#16005 = CARTESIAN_POINT ( 'NONE',  ( -12.69999999999999929, 0.000000000000000000, 0.000000000000000000 ) ) ;
#16006 = AXIS2_PLACEMENT_3D ( 'NONE', #1212, #7466, #522 ) ;
#16007 = EDGE_CURVE ( 'NONE', #4065, #12365, #3323, .T. ) ;
#16008 = AXIS2_PLACEMENT_3D ( 'NONE', #6408, #12406, #12212 ) ;
#16009 = CIRCLE ( 'NONE', #7791, 5.000000000000004441 ) ;
#16010 = ORIENTED_EDGE ( 'NONE', *, *, #5992, .T. ) ;
#16011 = CARTESIAN_POINT ( 'NONE',  ( 5.000000000000002665, 0.000000000000000000, -2.700000000000000622 ) ) ;
#16012 = DIRECTION ( 'NONE',  ( 0.000000000000000000, 0.000000000000000000, 1.000000000000000000 ) ) ;
#16013 = ORIENTED_EDGE ( 'NONE', *, *, #14134, .T. ) ;
#16014 = CARTESIAN_POINT ( 'NONE',  ( 32.50000000000000000, -30.00000000000000000, -2.649999999999631317 ) ) ;
#16015 = EDGE_CURVE ( 'NONE', #11247, #13167, #15154, .T. ) ;
#16016 = CARTESIAN_POINT ( 'NONE',  ( 0.000000000000000000, 31.97297851452424311, 46.27827401617415148 ) ) ;
#16017 = CARTESIAN_POINT ( 'NONE',  ( 10.00000000000000000, -56.37237871411034718, 1.017308535512174261 ) ) ;
#16018 = FACE_OUTER_BOUND ( 'NONE', #10285, .T. ) ;
#16019 = CIRCLE ( 'NONE', #7799, 24.00000000002399503 ) ;
#16020 = LINE ( 'NONE', #1546, #2607 ) ;
#16021 = ORIENTED_EDGE ( 'NONE', *, *, #342, .T. ) ;
#16022 = CARTESIAN_POINT ( 'NONE',  ( 10.00000000000000000, 0.000000000000000000, 0.000000000000000000 ) ) ;
#16023 = AXIS2_PLACEMENT_3D ( 'NONE', #17620, #4567, #7054 ) ;
#16024 = ORIENTED_EDGE ( 'NONE', *, *, #14798, .F. ) ;
#16025 = AXIS2_PLACEMENT_3D ( 'NONE', #4766, #6191, #1908 ) ;
#16026 = CARTESIAN_POINT ( 'NONE',  ( -11.25000000000000355, 29.90000000000000213, 0.000000000000000000 ) ) ;
#16027 = CARTESIAN_POINT ( 'NONE',  ( 0.000000000000000000, -55.33199130079790962, 10.11537145609357502 ) ) ;
#16028 = VERTEX_POINT ( 'NONE', #6674 ) ;
#16029 = TOROIDAL_SURFACE ( 'NONE', #6299, 25.10000000000000142, 0.09999999999999853451 ) ;
#16030 = CIRCLE ( 'NONE', #15421, 12.00000000001200462 ) ;
#16031 = APPLICATION_PROTOCOL_DEFINITION ( 'draft international standard', 'automotive_design', 1998, #16821 ) ;
#16032 = ORIENTED_EDGE ( 'NONE', *, *, #162, .F. ) ;
#16033 = AXIS2_PLACEMENT_3D ( 'NONE', #5013, #12263, #10822 ) ;
#16034 = VERTEX_POINT ( 'NONE', #9520 ) ;
#16035 = AXIS2_PLACEMENT_3D ( 'NONE', #16940, #2458, #14076 ) ;
#16036 = FACE_BOUND ( 'NONE', #3705, .T. ) ;
#16037 = DIRECTION ( 'NONE',  ( 0.000000000000000000, 0.000000000000000000, -1.000000000000000000 ) ) ;
#16038 = AXIS2_PLACEMENT_3D ( 'NONE', #15398, #12543, #9870 ) ;
#16039 = DIRECTION ( 'NONE',  ( 0.000000000000000000, -0.8090169943749402348, -0.5877852522924829071 ) ) ;
#16040 = ADVANCED_FACE ( 'NONE', ( #3633, #3722, #10846 ), #16672, .T. ) ;
#16041 = DIRECTION ( 'NONE',  ( -1.000000000000000000, 0.000000000000000000, 0.000000000000000000 ) ) ;
#16042 = CARTESIAN_POINT ( 'NONE',  ( -79.64793068852927149, -30.00000000000000000, 31.86039329588764701 ) ) ;
#16043 = LINE ( 'NONE', #3003, #12238 ) ;
#16044 = FACE_OUTER_BOUND ( 'NONE', #8770, .T. ) ;
#16045 = ORIENTED_EDGE ( 'NONE', *, *, #6542, .T. ) ;
#16046 = DIRECTION ( 'NONE',  ( -1.000000000000000000, 0.000000000000000000, 0.000000000000000000 ) ) ;
#16047 = CARTESIAN_POINT ( 'NONE',  ( 5.000000000000002665, 3.306546357697854226E-16, 2.700000000000000622 ) ) ;
#16048 = CARTESIAN_POINT ( 'NONE',  ( 10.00000000000000000, 20.41355805489615705, 19.44239304137382973 ) ) ;
#16049 = VECTOR ( 'NONE', #5596, 1000.000000000000000 ) ;
#16050 = ORIENTED_EDGE ( 'NONE', *, *, #10853, .F. ) ;
#16051 = ORIENTED_EDGE ( 'NONE', *, *, #14697, .F. ) ;
#16052 = DIRECTION ( 'NONE',  ( -1.000000000000000000, -0.000000000000000000, -0.000000000000000000 ) ) ;
#16053 = PRESENTATION_STYLE_ASSIGNMENT (( #4427 ) ) ;
#16054 = CIRCLE ( 'NONE', #15444, 2.041999999999999815 ) ;
#16055 = ORIENTED_EDGE ( 'NONE', *, *, #17493, .T. ) ;
#16056 = AXIS2_PLACEMENT_3D ( 'NONE', #1668, #14629, #4168 ) ;
#16057 = CONICAL_SURFACE ( 'NONE', #7831, 2.055000000000000160, 0.7853981633974794763 ) ;
#16058 = PRODUCT_DEFINITION_SHAPE ( 'NONE', 'NONE',  #18815 ) ;
#16059 = EDGE_CURVE ( 'NONE', #1905, #12396, #14046, .T. ) ;
#16060 = DIRECTION ( 'NONE',  ( 0.000000000000000000, 1.000000000000000000, -1.224646799147353207E-16 ) ) ;
#16061 = DIRECTION ( 'NONE',  ( 0.000000000000000000, -0.8090169943749401238, -0.5877852522924831291 ) ) ;
#16062 = VECTOR ( 'NONE', #1012, 1000.000000000000114 ) ;
#16063 = DIRECTION ( 'NONE',  ( -1.000000000000000000, 0.000000000000000000, 0.000000000000000000 ) ) ;
#16064 = VERTEX_POINT ( 'NONE', #13807 ) ;
#16065 = CARTESIAN_POINT ( 'NONE',  ( 0.000000000000000000, 0.000000000000000000, 0.000000000000000000 ) ) ;
#16066 = AXIS2_PLACEMENT_3D ( 'NONE', #15373, #8146, #12523 ) ;
#16067 = ORIENTED_EDGE ( 'NONE', *, *, #3264, .T. ) ;
#16068 = PRODUCT_DEFINITION_CONTEXT ( 'detailed design', #12172, 'design' ) ;
#16069 = CIRCLE ( 'NONE', #7855, 26.24900000002624978 ) ;
#16070 = DIRECTION ( 'NONE',  ( 0.000000000000000000, 0.000000000000000000, 1.000000000000000000 ) ) ;
#16071 = ORIENTED_EDGE ( 'NONE', *, *, #1330, .F. ) ;
#16072 = ORIENTED_EDGE ( 'NONE', *, *, #16455, .T. ) ;
#16073 = DIRECTION ( 'NONE',  ( 0.000000000000000000, -0.3090169943749546677, 0.9510565162951511997 ) ) ;
#16074 = CARTESIAN_POINT ( 'NONE',  ( 0.000000000000000000, -50.69000562871659810, 24.68609584167141691 ) ) ;
#16075 = EDGE_LOOP ( 'NONE', ( #17473, #2342, #13879, #6589 ) ) ;
#16076 = ORIENTED_EDGE ( 'NONE', *, *, #9943, .F. ) ;
#16077 = CARTESIAN_POINT ( 'NONE',  ( -90.00000000009001155, -88.00000000000000000, -1.301042606982603940E-15 ) ) ;
#16078 = ORIENTED_EDGE ( 'NONE', *, *, #13194, .T. ) ;
#16079 = LINE ( 'NONE', #3215, #6360 ) ;
#16080 = VECTOR ( 'NONE', #11062, 1000.000000000000000 ) ;
#16081 = AXIS2_PLACEMENT_3D ( 'NONE', #8223, #6496, #12498 ) ;
#16082 = AXIS2_PLACEMENT_3D ( 'NONE', #6084, #16468, #17615 ) ;
#16083 = CARTESIAN_POINT ( 'NONE',  ( -17.77999999999999758, 0.000000000000000000, 0.000000000000000000 ) ) ;
#16084 = ORIENTED_EDGE ( 'NONE', *, *, #6917, .T. ) ;
#16085 = AXIS2_PLACEMENT_3D ( 'NONE', #9748, #9929, #17092 ) ;
#16086 = ORIENTED_EDGE ( 'NONE', *, *, #4005, .T. ) ;
#16087 = DIRECTION ( 'NONE',  ( -0.000000000000000000, 1.000000000000000000, -0.000000000000000000 ) ) ;
#16088 = DIRECTION ( 'NONE',  ( -1.000000000000000000, -0.000000000000000000, 0.000000000000000000 ) ) ;
#16089 = DIRECTION ( 'NONE',  ( 0.000000000000000000, 0.000000000000000000, -1.000000000000000000 ) ) ;
#16090 = ORIENTED_EDGE ( 'NONE', *, *, #13416, .F. ) ;
#16091 = DIRECTION ( 'NONE',  ( -1.000000000000000000, -0.000000000000000000, 0.000000000000000000 ) ) ;
#16092 = AXIS2_PLACEMENT_3D ( 'NONE', #5428, #15806, #8642 ) ;
#16093 = CARTESIAN_POINT ( 'NONE',  ( -117.1020693116508085, -34.99999999999999289, 17.04080595179778967 ) ) ;
#16094 = CARTESIAN_POINT ( 'NONE',  ( 10.00000000000000000, 0.000000000000000000, 0.000000000000000000 ) ) ;
#16095 = CARTESIAN_POINT ( 'NONE',  ( -23.50000000000000355, 2.877919977996280715E-15, -2.000000000000000000 ) ) ;
#16096 = ORIENTED_EDGE ( 'NONE', *, *, #6488, .F. ) ;
#16097 = AXIS2_PLACEMENT_3D ( 'NONE', #14543, #4114, #4180 ) ;
#16098 = DIRECTION ( 'NONE',  ( 0.000000000000000000, -0.1564344650402381964, 0.9876883405951365491 ) ) ;
#16099 = EDGE_CURVE ( 'NONE', #18692, #16028, #8793, .T. ) ;
#16100 = DIRECTION ( 'NONE',  ( -0.000000000000000000, -1.000000000000000000, -0.000000000000000000 ) ) ;
#16101 = ADVANCED_FACE ( 'NONE', ( #12478 ), #16860, .T. ) ;
#16102 = VERTEX_POINT ( 'NONE', #15529 ) ;
#16103 = FACE_BOUND ( 'NONE', #13749, .T. ) ;
#16104 = DIRECTION ( 'NONE',  ( 0.000000000000000000, 0.000000000000000000, 1.000000000000000000 ) ) ;
#16105 = EDGE_CURVE ( 'NONE', #2267, #2260, #6041, .T. ) ;
#16106 = AXIS2_PLACEMENT_3D ( 'NONE', #10760, #18100, #15252 ) ;
#16107 = AXIS2_PLACEMENT_3D ( 'NONE', #9867, #2534, #15679 ) ;
#16108 = EDGE_CURVE ( 'NONE', #5435, #2351, #11241, .T. ) ;
#16109 = VERTEX_POINT ( 'NONE', #6850 ) ;
#16110 = CARTESIAN_POINT ( 'NONE',  ( 20.55500000000001748, 0.000000000000000000, 0.000000000000000000 ) ) ;
#16111 = DIRECTION ( 'NONE',  ( -1.000000000000000000, -0.000000000000000000, 0.000000000000000000 ) ) ;
#16112 = ADVANCED_FACE ( 'NONE', ( #17246 ), #8, .T. ) ;
#16113 = EDGE_LOOP ( 'NONE', ( #14427, #2426, #17689, #16159, #2379 ) ) ;
#16114 = LINE ( 'NONE', #3068, #6598 ) ;
#16115 = CARTESIAN_POINT ( 'NONE',  ( 0.000000000000000000, 2.357898499370432166, -2.385244779468109755E-15 ) ) ;
#16116 = AXIS2_PLACEMENT_3D ( 'NONE', #7516, #17706, #11982 ) ;
#16117 = FACE_OUTER_BOUND ( 'NONE', #18681, .T. ) ;
#16118 = DIRECTION ( 'NONE',  ( 0.000000000000000000, 0.000000000000000000, 1.000000000000000000 ) ) ;
#16119 = ORIENTED_EDGE ( 'NONE', *, *, #11285, .F. ) ;
#16120 = DIRECTION ( 'NONE',  ( -1.000000000000000000, -0.000000000000000000, 0.000000000000000000 ) ) ;
#16121 = ORIENTED_EDGE ( 'NONE', *, *, #9442, .F. ) ;
#16122 = EDGE_CURVE ( 'NONE', #15432, #12639, #16980, .T. ) ;
#16123 = CIRCLE ( 'NONE', #17952, 63.00000000006298961 ) ;
#16124 = ADVANCED_FACE ( 'NONE', ( #18477 ), #2710, .T. ) ;
#16125 = SURFACE_STYLE_USAGE ( .BOTH. , #4871 ) ;
#16126 = DIRECTION ( 'NONE',  ( -1.000000000000000000, 0.000000000000000000, -0.000000000000000000 ) ) ;
#16127 = VERTEX_POINT ( 'NONE', #2854 ) ;
#16128 = APPLICATION_PROTOCOL_DEFINITION ( 'draft international standard', 'automotive_design', 1998, #14979 ) ;
#16129 = EDGE_CURVE ( 'NONE', #432, #17588, #10904, .T. ) ;
#16130 = ORIENTED_EDGE ( 'NONE', *, *, #11592, .T. ) ;
#16131 = EDGE_CURVE ( 'NONE', #18131, #2367, #15619, .T. ) ;
#16132 = SHAPE_REPRESENTATION ( 'Indexing Ring', ( #8017 ), #15633 ) ;
#16133 = AXIS2_PLACEMENT_3D ( 'NONE', #7280, #16138, #3000 ) ;
#16134 = CIRCLE ( 'NONE', #8241, 6.080745460913608902 ) ;
#16135 = CYLINDRICAL_SURFACE ( 'NONE', #510, 26.24900000002624978 ) ;
#16136 = LINE ( 'NONE', #13373, #2760 ) ;
#16137 = DIRECTION ( 'NONE',  ( 0.000000000000000000, 0.000000000000000000, 1.000000000000000000 ) ) ;
#16138 = DIRECTION ( 'NONE',  ( -1.000000000000000000, -0.000000000000000000, -0.000000000000000000 ) ) ;
#16139 = FACE_OUTER_BOUND ( 'NONE', #5198, .T. ) ;
#16140 = CARTESIAN_POINT ( 'NONE',  ( 10.00000000000000000, 55.83748330407397020, 7.813799127874245798 ) ) ;
#16141 = DIRECTION ( 'NONE',  ( 0.000000000000000000, 1.000000000000000000, 0.000000000000000000 ) ) ;
#16142 = ORIENTED_EDGE ( 'NONE', *, *, #11896, .F. ) ;
#16143 =( NAMED_UNIT ( * ) SI_UNIT ( $, .STERADIAN. ) SOLID_ANGLE_UNIT ( ) );
#16144 = CARTESIAN_POINT ( 'NONE',  ( 0.000000000000000000, 62.72529079327807011, 5.876895005582658982 ) ) ;
#16145 = LINE ( 'NONE', #13566, #17290 ) ;
#16146 = EDGE_LOOP ( 'NONE', ( #1444, #798, #3853, #12706 ) ) ;
#16147 = EDGE_LOOP ( 'NONE', ( #4243, #131, #3202, #11003 ) ) ;
#16148 = LINE ( 'NONE', #1755, #4444 ) ;
#16149 = AXIS2_PLACEMENT_3D ( 'NONE', #2451, #1028, #16393 ) ;
#16150 =( NAMED_UNIT ( * ) SI_UNIT ( $, .STERADIAN. ) SOLID_ANGLE_UNIT ( ) );
#16151 = DIRECTION ( 'NONE',  ( -1.000000000000000000, -0.000000000000000000, -0.000000000000000000 ) ) ;
#16152 = ORIENTED_EDGE ( 'NONE', *, *, #7718, .T. ) ;
#16153 = EDGE_CURVE ( 'NONE', #15934, #16801, #4375, .T. ) ;
#16154 = CARTESIAN_POINT ( 'NONE',  ( 10.00000000000000000, -55.83748330407401284, -7.813799127873885197 ) ) ;
#16155 = CARTESIAN_POINT ( 'NONE',  ( 0.5469614295415388128, -4.303013824935362663, -3.535263753543555598 ) ) ;
#16156 = CARTESIAN_POINT ( 'NONE',  ( -26.29305231718584324, -34.99999999999999289, 21.75302069950530637 ) ) ;
#16157 = ORIENTED_EDGE ( 'NONE', *, *, #9915, .F. ) ;
#16158 = FACE_OUTER_BOUND ( 'NONE', #11517, .T. ) ;
#16159 = ORIENTED_EDGE ( 'NONE', *, *, #11896, .T. ) ;
#16160 = DIRECTION ( 'NONE',  ( -1.000000000000000000, 0.000000000000000000, 0.000000000000000000 ) ) ;
#16161 = EDGE_LOOP ( 'NONE', ( #9590, #3211, #12884 ) ) ;
#16162 = EDGE_CURVE ( 'NONE', #13701, #1626, #2563, .T. ) ;
#16163 = CARTESIAN_POINT ( 'NONE',  ( -36.40576474687271258, 10.00000000000000000, -23.80033635316118890 ) ) ;
#16164 = CYLINDRICAL_SURFACE ( 'NONE', #10417, 28.00000000000000355 ) ;
#16165 = VERTEX_POINT ( 'NONE', #12865 ) ;
#16166 = ORIENTED_EDGE ( 'NONE', *, *, #524, .F. ) ;
#16167 = DIRECTION ( 'NONE',  ( -1.000000000000000000, 0.000000000000000000, 0.000000000000000000 ) ) ;
#16168 = EDGE_CURVE ( 'NONE', #14997, #4430, #12770, .T. ) ;
#16169 = VERTEX_POINT ( 'NONE', #8380 ) ;
#16170 = DIRECTION ( 'NONE',  ( -1.000000000000000000, 0.000000000000000000, 0.000000000000000000 ) ) ;
#16171 = AXIS2_PLACEMENT_3D ( 'NONE', #10224, #11932, #16225 ) ;
#16172 = AXIS2_PLACEMENT_3D ( 'NONE', #1720, #14678, #308 ) ;
#16173 = FACE_OUTER_BOUND ( 'NONE', #1824, .T. ) ;
#16174 = AXIS2_PLACEMENT_3D ( 'NONE', #6841, #12658, #14180 ) ;
#16175 = ORIENTED_EDGE ( 'NONE', *, *, #17170, .F. ) ;
#16176 = ORIENTED_EDGE ( 'NONE', *, *, #13457, .T. ) ;
#16177 = CARTESIAN_POINT ( 'NONE',  ( 10.00000000000000000, -55.74967257055877212, -7.478235706489567924 ) ) ;
#16178 = PLANE ( 'NONE',  #7748 ) ;
#16179 = CARTESIAN_POINT ( 'NONE',  ( 10.00000000000000000, 0.000000000000000000, 0.000000000000000000 ) ) ;
#16180 = EDGE_CURVE ( 'NONE', #657, #2530, #4238, .T. ) ;
#16181 = ORIENTED_EDGE ( 'NONE', *, *, #17845, .T. ) ;
#16182 = DIRECTION ( 'NONE',  ( 0.000000000000000000, 0.000000000000000000, 1.000000000000000000 ) ) ;
#16183 = DIRECTION ( 'NONE',  ( -2.031314180040284764E-16, -1.000000000000000000, -1.301042606982601377E-16 ) ) ;
#16184 = DIRECTION ( 'NONE',  ( 0.000000000000000000, 0.000000000000000000, 1.000000000000000000 ) ) ;
#16185 = CARTESIAN_POINT ( 'NONE',  ( 0.000000000000000000, 27.94286728106393269, 3.730438010304423013 ) ) ;
#16186 = ORIENTED_EDGE ( 'NONE', *, *, #427, .F. ) ;
#16187 = CARTESIAN_POINT ( 'NONE',  ( 2.500000000000000000, 2.357898499370432166, -2.385244779468109755E-15 ) ) ;
#16188 = DIRECTION ( 'NONE',  ( 0.000000000000000000, 0.000000000000000000, -1.000000000000000000 ) ) ;
#16189 = EDGE_CURVE ( 'NONE', #14103, #1805, #894, .T. ) ;
#16190 = VECTOR ( 'NONE', #8386, 1000.000000000000000 ) ;
#16191 = VERTEX_POINT ( 'NONE', #5715 ) ;
#16192 = CARTESIAN_POINT ( 'NONE',  ( 0.000000000000000000, 53.89344778774812283, 16.10733642026502110 ) ) ;
#16193 = DIRECTION ( 'NONE',  ( 0.000000000000000000, 0.000000000000000000, 1.000000000000000000 ) ) ;
#16194 = ADVANCED_FACE ( 'NONE', ( #18664 ), #5439, .T. ) ;
#16195 = ORIENTED_EDGE ( 'NONE', *, *, #8562, .F. ) ;
#16197 = CARTESIAN_POINT ( 'NONE',  ( 21.00000000000000355, 0.000000000000000000, 0.000000000000000000 ) ) ;
#16196 = CIRCLE ( 'NONE', #2203, 24.00000000002400569 ) ;
#16198 = ADVANCED_FACE ( 'NONE', ( #11530 ), #4290, .T. ) ;
#16199 = LINE ( 'NONE', #3152, #8250 ) ;
#16200 = CIRCLE ( 'NONE', #12871, 25.00000000000000355 ) ;
#16201 = VERTEX_POINT ( 'NONE', #1422 ) ;
#16202 = LINE ( 'NONE', #7530, #13056 ) ;
#16203 =( REPRESENTATION_RELATIONSHIP ('NONE','NONE', #11014, #8256 ) REPRESENTATION_RELATIONSHIP_WITH_TRANSFORMATION ( #13458 )SHAPE_REPRESENTATION_RELATIONSHIP( ) );
#16204 = CARTESIAN_POINT ( 'NONE',  ( 11.25000000000000000, 0.000000000000000000, 29.90000000000000213 ) ) ;
#16205 = PRODUCT_RELATED_PRODUCT_CATEGORY ( 'part', '', ( #15589 ) ) ;
#16206 = CARTESIAN_POINT ( 'NONE',  ( 10.00000000000000000, 41.62350880771921169, 47.29147401531969308 ) ) ;
#16207 = CARTESIAN_POINT ( 'NONE',  ( 0.000000000000000000, 10.00000000000000000, -150.0000000000000284 ) ) ;
#16208 = DIRECTION ( 'NONE',  ( 1.000000000000000000, 0.000000000000000000, 0.000000000000000000 ) ) ;
#16209 = ORIENTED_EDGE ( 'NONE', *, *, #12967, .F. ) ;
#16210 = CARTESIAN_POINT ( 'NONE',  ( -90.00000000009001155, -34.99999999999999289, -1.301042606982603940E-15 ) ) ;
#16211 = ORIENTED_EDGE ( 'NONE', *, *, #11018, .T. ) ;
#16212 = FACE_OUTER_BOUND ( 'NONE', #5923, .T. ) ;
#16213 = ORIENTED_EDGE ( 'NONE', *, *, #15242, .T. ) ;
#16214 = VECTOR ( 'NONE', #18248, 1000.000000000000000 ) ;
#16215 = ORIENTED_EDGE ( 'NONE', *, *, #4086, .F. ) ;
#16216 = EDGE_CURVE ( 'NONE', #15951, #6735, #15965, .T. ) ;
#16217 = ORIENTED_EDGE ( 'NONE', *, *, #8931, .F. ) ;
#16218 = ADVANCED_FACE ( 'NONE', ( #5804 ), #10276, .T. ) ;
#16219 = ORIENTED_EDGE ( 'NONE', *, *, #5736, .T. ) ;
#16220 = DIRECTION ( 'NONE',  ( -1.000000000000000000, 0.000000000000000000, 0.000000000000000000 ) ) ;
#16221 = EDGE_CURVE ( 'NONE', #2222, #17488, #1372, .T. ) ;
#16222 = EDGE_CURVE ( 'NONE', #125, #91, #11802, .T. ) ;
#16223 = CARTESIAN_POINT ( 'NONE',  ( 10.00000000000000000, 42.79754323328179311, -13.90576474687299680 ) ) ;
#16224 = DIRECTION ( 'NONE',  ( 0.000000000000000000, 1.000000000000000000, 3.469446951950144779E-15 ) ) ;
#16225 = DIRECTION ( 'NONE',  ( 0.000000000000000000, 0.000000000000000000, 1.000000000000000000 ) ) ;
#16226 = VECTOR ( 'NONE', #15468, 1000.000000000000000 ) ;
#16227 = EDGE_CURVE ( 'NONE', #9439, #12674, #8669, .T. ) ;
#16228 = DIRECTION ( 'NONE',  ( 0.000000000000000000, 0.000000000000000000, -1.000000000000000000 ) ) ;
#16229 = DIRECTION ( 'NONE',  ( 1.000000000000000000, 0.000000000000000000, 0.000000000000000000 ) ) ;
#16230 = CARTESIAN_POINT ( 'NONE',  ( 10.00000000000000000, -20.41355805489602204, -19.44239304137396118 ) ) ;
#16231 = CYLINDRICAL_SURFACE ( 'NONE', #575, 63.00000000006298961 ) ;
#16232 = ORIENTED_EDGE ( 'NONE', *, *, #17782, .T. ) ;
#16233 = SURFACE_STYLE_USAGE ( .BOTH. , #1650 ) ;
#16234 = DIRECTION ( 'NONE',  ( -1.000000000000000000, 0.000000000000000000, -0.000000000000000000 ) ) ;
#16235 = CARTESIAN_POINT ( 'NONE',  ( 10.04305231718605285, -26.50000000000000000, -28.25933677959240953 ) ) ;
#16236 = ORIENTED_EDGE ( 'NONE', *, *, #10055, .F. ) ;
#16237 = VERTEX_POINT ( 'NONE', #7603 ) ;
#16238 = CARTESIAN_POINT ( 'NONE',  ( 0.000000000000000000, 20.32630374611208879, -16.60877409751146416 ) ) ;
#16239 = ADVANCED_FACE ( 'NONE', ( #1519 ), #454, .T. ) ;
#16240 = CARTESIAN_POINT ( 'NONE',  ( 10.00000000000000000, -32.46095361140696411, 5.940243314904091854 ) ) ;
#16241 = ORIENTED_EDGE ( 'NONE', *, *, #12252, .T. ) ;
#16242 = ADVANCED_FACE ( 'NONE', ( #5982, #7321 ), #14654, .T. ) ;
#16243 = LINE ( 'NONE', #7576, #2905 ) ;
#16244 = CARTESIAN_POINT ( 'NONE',  ( 5.000000000000000000, -47.29147401531926675, -41.62350880771970196 ) ) ;
#16245 = LINE ( 'NONE', #2055, #1740 ) ;
#16246 = ORIENTED_EDGE ( 'NONE', *, *, #17629, .F. ) ;
#16247 = CARTESIAN_POINT ( 'NONE',  ( 10.00000000000000000, 20.41355805489643060, -19.44239304137353841 ) ) ;
#16248 = ORIENTED_EDGE ( 'NONE', *, *, #3612, .F. ) ;
#16249 = FACE_OUTER_BOUND ( 'NONE', #2366, .T. ) ;
#16250 = VERTEX_POINT ( 'NONE', #13422 ) ;
#16251 = ADVANCED_FACE ( 'NONE', ( #4647 ), #16178, .F. ) ;
#16252 =( GEOMETRIC_REPRESENTATION_CONTEXT ( 3 ) GLOBAL_UNCERTAINTY_ASSIGNED_CONTEXT ( ( #17018 ) ) GLOBAL_UNIT_ASSIGNED_CONTEXT ( ( #2840, #13217, #13037 ) ) REPRESENTATION_CONTEXT ( 'NONE', 'WORKASPACE' ) );
#16253 = DIRECTION ( 'NONE',  ( -1.000000000000000000, -0.000000000000000000, -0.000000000000000000 ) ) ;
#16254 = CARTESIAN_POINT ( 'NONE',  ( -4.236525694536558362, 2.416953475386465211, -3.751298745799836354 ) ) ;
#16255 = ORIENTED_EDGE ( 'NONE', *, *, #18010, .F. ) ;
#16256 = VERTEX_POINT ( 'NONE', #16373 ) ;
#16257 = DIRECTION ( 'NONE',  ( -0.000000000000000000, 1.000000000000000000, -0.000000000000000000 ) ) ;
#16258 = FILL_AREA_STYLE ('',( #11516 ) ) ;
#16259 = ORIENTED_EDGE ( 'NONE', *, *, #9100, .F. ) ;
#16260 = CARTESIAN_POINT ( 'NONE',  ( 10.00000000000000000, 0.000000000000000000, 0.000000000000000000 ) ) ;
#16261 = CARTESIAN_POINT ( 'NONE',  ( -4.024497503033714452, 2.323544716729487813, -3.572167766733750582 ) ) ;
#16262 = CIRCLE ( 'NONE', #2890, 24.00000000002399858 ) ;
#16263 = ORIENTED_EDGE ( 'NONE', *, *, #15287, .F. ) ;
#16264 = ORIENTED_EDGE ( 'NONE', *, *, #3078, .T. ) ;
#16265 = DIRECTION ( 'NONE',  ( -1.000000000000000000, 0.000000000000000000, -0.000000000000000000 ) ) ;
#16266 = DIRECTION ( 'NONE',  ( 0.000000000000000000, 0.000000000000000000, 1.000000000000000000 ) ) ;
#16267 = DIRECTION ( 'NONE',  ( -1.000000000000000000, 0.000000000000000000, 0.000000000000000000 ) ) ;
#16268 = VERTEX_POINT ( 'NONE', #4844 ) ;
#16269 = DIRECTION ( 'NONE',  ( 0.000000000000000000, 0.000000000000000000, 1.000000000000000000 ) ) ;
#16270 = EDGE_CURVE ( 'NONE', #6404, #10818, #4708, .T. ) ;
#16271 = CARTESIAN_POINT ( 'NONE',  ( 11.14999999999999680, 0.000000000000000000, 25.00000000000000355 ) ) ;
#16272 = DIRECTION ( 'NONE',  ( 0.000000000000000000, 0.000000000000000000, 1.000000000000000000 ) ) ;
#16273 = LINE ( 'NONE', #17520, #5668 ) ;
#16274 = VERTEX_POINT ( 'NONE', #4466 ) ;
#16275 = CARTESIAN_POINT ( 'NONE',  ( 10.00000000000000000, 9.823366686501460165, -55.51919907100641893 ) ) ;
#16276 =( LENGTH_UNIT ( ) NAMED_UNIT ( * ) SI_UNIT ( .MILLI., .METRE. ) );
#16277 = CARTESIAN_POINT ( 'NONE',  ( 4.144923636027600722, -29.35885059145708098, -2.000000000000000000 ) ) ;
#16278 = VERTEX_POINT ( 'NONE', #17890 ) ;
#16279 = FACE_OUTER_BOUND ( 'NONE', #15986, .T. ) ;
#16280 = CARTESIAN_POINT ( 'NONE',  ( 10.00000000000000000, -1.489278925039337453, -26.20671763660629949 ) ) ;
#16281 = AXIS2_PLACEMENT_3D ( 'NONE', #13978, #1123, #2448 ) ;
#16282 = VECTOR ( 'NONE', #8320, 1000.000000000000000 ) ;
#16283 = ADVANCED_FACE ( 'NONE', ( #4737 ), #10450, .T. ) ;
#16284 = ORIENTED_EDGE ( 'NONE', *, *, #14323, .T. ) ;
#16285 = ADVANCED_FACE ( 'NONE', ( #14846 ), #6079, .T. ) ;
#16286 = DIRECTION ( 'NONE',  ( -1.000000000000000000, 0.000000000000000000, 0.000000000000000000 ) ) ;
#16287 = CARTESIAN_POINT ( 'NONE',  ( -79.64793068852898728, -30.00000000000000000, -31.86039329588756530 ) ) ;
#16288 = AXIS2_PLACEMENT_3D ( 'NONE', #15397, #8167, #2911 ) ;
#16289 = ORIENTED_EDGE ( 'NONE', *, *, #8259, .F. ) ;
#16290 =( NAMED_UNIT ( * ) SI_UNIT ( $, .STERADIAN. ) SOLID_ANGLE_UNIT ( ) );
#16291 = CIRCLE ( 'NONE', #4751, 0.2500000000000002220 ) ;
#16292 = LINE ( 'NONE', #3154, #9609 ) ;
#16293 = DIRECTION ( 'NONE',  ( 0.000000000000000000, 0.000000000000000000, 1.000000000000000000 ) ) ;
#16294 = CARTESIAN_POINT ( 'NONE',  ( -90.00000000009001155, -49.14213562373095812, -1.301042606982603940E-15 ) ) ;
#16295 = DIRECTION ( 'NONE',  ( 1.000000000000000000, 0.000000000000000000, 0.000000000000000000 ) ) ;
#16296 = ORIENTED_EDGE ( 'NONE', *, *, #4432, .T. ) ;
#16297 = FACE_OUTER_BOUND ( 'NONE', #1396, .T. ) ;
#16298 = ORIENTED_EDGE ( 'NONE', *, *, #5402, .T. ) ;
#16299 = DIRECTION ( 'NONE',  ( 0.000000000000000000, 0.000000000000000000, -1.000000000000000000 ) ) ;
#16300 = ORIENTED_EDGE ( 'NONE', *, *, #15893, .T. ) ;
#16301 = AXIS2_PLACEMENT_3D ( 'NONE', #12445, #11001, #17116 ) ;
#16302 = AXIS2_PLACEMENT_3D ( 'NONE', #11581, #12723, #5772 ) ;
#16303 = CONTEXT_DEPENDENT_SHAPE_REPRESENTATION ( #1956, #15005 ) ;
#16304 = AXIS2_PLACEMENT_3D ( 'NONE', #5641, #3831, #5462 ) ;
#16305 = VERTEX_POINT ( 'NONE', #9126 ) ;
#16306 = AXIS2_PLACEMENT_3D ( 'NONE', #12521, #12427, #10986 ) ;
#16307 = AXIS2_PLACEMENT_3D ( 'NONE', #17385, #12911, #2621 ) ;
#16308 = ORIENTED_EDGE ( 'NONE', *, *, #15431, .T. ) ;
#16309 = VERTEX_POINT ( 'NONE', #95 ) ;
#16310 = DIRECTION ( 'NONE',  ( -1.000000000000000000, 0.000000000000000000, 0.000000000000000000 ) ) ;
#16311 = CYLINDRICAL_SURFACE ( 'NONE', #9422, 24.00000000002399858 ) ;
#16312 = AXIS2_PLACEMENT_3D ( 'NONE', #13235, #10101, #15912 ) ;
#16313 = CARTESIAN_POINT ( 'NONE',  ( 10.00000000000000000, -56.37237871411034718, 25.01730853553617351 ) ) ;
#16314 = CARTESIAN_POINT ( 'NONE',  ( 0.000000000000000000, 11.24999999999999467, 0.000000000000000000 ) ) ;
#16315 = AXIS2_PLACEMENT_3D ( 'NONE', #15720, #2475, #5233 ) ;
#16316 = CYLINDRICAL_SURFACE ( 'NONE', #6300, 2.649999999999999467 ) ;
#16317 = DIRECTION ( 'NONE',  ( -1.000000000000000000, 0.000000000000000000, -0.000000000000000000 ) ) ;
#16318 = VECTOR ( 'NONE', #17083, 1000.000000000000000 ) ;
#16319 = FACE_OUTER_BOUND ( 'NONE', #11443, .T. ) ;
#16320 = CIRCLE ( 'NONE', #8113, 26.24900000002624978 ) ;
#16321 = CARTESIAN_POINT ( 'NONE',  ( 10.00000000000000000, -32.46095361140688595, -5.940243314904558147 ) ) ;
#16322 = ORIENTED_EDGE ( 'NONE', *, *, #395, .T. ) ;
#16323 = LINE ( 'NONE', #516, #6566 ) ;
#16324 = CARTESIAN_POINT ( 'NONE',  ( -12.69999999999999929, 0.000000000000000000, 0.000000000000000000 ) ) ;
#16325 = DIRECTION ( 'NONE',  ( -1.000000000000000000, 0.000000000000000000, 0.000000000000000000 ) ) ;
#16326 = VERTEX_POINT ( 'NONE', #8927 ) ;
#16327 = ORIENTED_EDGE ( 'NONE', *, *, #2202, .T. ) ;
#16328 = EDGE_CURVE ( 'NONE', #17285, #16305, #362, .T. ) ;
#16329 = EDGE_CURVE ( 'NONE', #7239, #16626, #11884, .T. ) ;
#16330 = DIRECTION ( 'NONE',  ( -1.000000000000000000, -0.000000000000000000, -0.000000000000000000 ) ) ;
#16331 = CARTESIAN_POINT ( 'NONE',  ( 13.90576474687263264, 15.00000000000001599, -42.79754323328189969 ) ) ;
#16333 = EDGE_CURVE ( 'NONE', #6635, #7978, #7684, .T. ) ;
#16332 = DIRECTION ( 'NONE',  ( 1.000000000000000000, 0.000000000000000000, 0.000000000000000000 ) ) ;
#16334 = VERTEX_POINT ( 'NONE', #13510 ) ;
#16335 = AXIS2_PLACEMENT_3D ( 'NONE', #2948, #17341, #12864 ) ;
#16336 = VECTOR ( 'NONE', #365, 1000.000000000000000 ) ;
#16337 = EDGE_CURVE ( 'NONE', #2762, #11035, #6233, .T. ) ;
#16338 = AXIS2_PLACEMENT_3D ( 'NONE', #9686, #14067, #7015 ) ;
#16339 = VECTOR ( 'NONE', #2564, 1000.000000000000000 ) ;
#16340 = EDGE_CURVE ( 'NONE', #4319, #17432, #12001, .T. ) ;
#16341 = CYLINDRICAL_SURFACE ( 'NONE', #15070, 24.00000000002399858 ) ;
#16342 = FACE_OUTER_BOUND ( 'NONE', #5156, .T. ) ;
#16343 = FACE_OUTER_BOUND ( 'NONE', #10168, .T. ) ;
#16344 = ORIENTED_EDGE ( 'NONE', *, *, #5107, .T. ) ;
#16345 = DIRECTION ( 'NONE',  ( 0.000000000000000000, 0.000000000000000000, -1.000000000000000000 ) ) ;
#16346 = EDGE_CURVE ( 'NONE', #8902, #13109, #14437, .T. ) ;
#16347 = AXIS2_PLACEMENT_3D ( 'NONE', #13050, #11618, #2951 ) ;
#16348 = ORIENTED_EDGE ( 'NONE', *, *, #1094, .F. ) ;
#16349 = FACE_OUTER_BOUND ( 'NONE', #6487, .T. ) ;
#16350 = EDGE_LOOP ( 'NONE', ( #10458, #11722, #3775, #16298 ) ) ;
#16351 = CIRCLE ( 'NONE', #6916, 63.00000000006298961 ) ;
#16352 = LINE ( 'NONE', #17592, #11441 ) ;
#16353 = DIRECTION ( 'NONE',  ( 0.000000000000000000, 0.000000000000000000, 1.000000000000000000 ) ) ;
#16354 = VECTOR ( 'NONE', #4990, 1000.000000000000000 ) ;
#16355 = EDGE_LOOP ( 'NONE', ( #16241, #7795, #16935, #6306, #14619, #12467 ) ) ;
#16356 = VERTEX_POINT ( 'NONE', #655 ) ;
#16357 = AXIS2_PLACEMENT_3D ( 'NONE', #9835, #8122, #12696 ) ;
#16358 = EDGE_CURVE ( 'NONE', #4068, #16268, #2274, .T. ) ;
#16359 = CARTESIAN_POINT ( 'NONE',  ( 0.000000000000000000, -54.20017844242534721, 32.11449294037177538 ) ) ;
#16360 = SURFACE_SIDE_STYLE ('',( #15022 ) ) ;
#16361 = ORIENTED_EDGE ( 'NONE', *, *, #11424, .T. ) ;
#16362 = CARTESIAN_POINT ( 'NONE',  ( 0.000000000000000000, -55.33199130079777461, -10.11537145609435306 ) ) ;
#16363 = AXIS2_PLACEMENT_3D ( 'NONE', #9409, #9693, #5304 ) ;
#16364 = EDGE_CURVE ( 'NONE', #10759, #9272, #4110, .T. ) ;
#16365 = AXIS2_PLACEMENT_3D ( 'NONE', #6418, #14996, #8895 ) ;
#16366 = CARTESIAN_POINT ( 'NONE',  ( 10.00000000000000000, 34.13306034420251223, -44.70888270294124567 ) ) ;
#16367 = CIRCLE ( 'NONE', #8157, 55.00000000000000000 ) ;
#16368 = AXIS2_PLACEMENT_3D ( 'NONE', #17249, #10281, #5809 ) ;
#16369 = ORIENTED_EDGE ( 'NONE', *, *, #10636, .T. ) ;
#16370 = PRODUCT_DEFINITION_SHAPE ( 'NONE', 'NONE',  #18831 ) ;
#16371 = VERTEX_POINT ( 'NONE', #16652 ) ;
#16372 = DIRECTION ( 'NONE',  ( 1.000000000000000000, 0.000000000000000000, -0.000000000000000000 ) ) ;
#16373 = CARTESIAN_POINT ( 'NONE',  ( 0.000000000000000000, -29.03656532225551601, -15.68049343256028294 ) ) ;
#16374 = CARTESIAN_POINT ( 'NONE',  ( 3.061616997868383043E-15, -26.50000000000000000, -25.00000000000000000 ) ) ;
#16375 = ORIENTED_EDGE ( 'NONE', *, *, #67, .F. ) ;
#16376 = CARTESIAN_POINT ( 'NONE',  ( 3.383466608491643077E-15, 4.736522675502341073, -3.681124513963742739 ) ) ;
#16377 = CARTESIAN_POINT ( 'NONE',  ( 5.000000000000000000, 48.50907078259439942, -40.19788616105557111 ) ) ;
#16378 = LINE ( 'NONE', #5017, #6467 ) ;
#16379 = AXIS2_PLACEMENT_3D ( 'NONE', #9388, #15208, #2151 ) ;
#16380 = DIRECTION ( 'NONE',  ( -1.000000000000000000, 0.000000000000000000, 0.000000000000000000 ) ) ;
#16381 = ORIENTED_EDGE ( 'NONE', *, *, #630, .F. ) ;
#16382 = DIRECTION ( 'NONE',  ( -1.000000000000000000, 0.000000000000000000, -0.000000000000000000 ) ) ;
#16383 = CARTESIAN_POINT ( 'NONE',  ( -87.43997332177200121, -14.11572627500821042, 6.475821446449874230 ) ) ;
#16384 = CIRCLE ( 'NONE', #2385, 0.1000000000000028644 ) ;
#16385 = ORIENTED_EDGE ( 'NONE', *, *, #5629, .F. ) ;
#16386 = LINE ( 'NONE', #17527, #17007 ) ;
#16387 = LINE ( 'NONE', #3345, #8613 ) ;
#16388 = AXIS2_PLACEMENT_3D ( 'NONE', #11638, #4394, #14216 ) ;
#16389 = EDGE_CURVE ( 'NONE', #13820, #4463, #9210, .T. ) ;
#16390 = AXIS2_PLACEMENT_3D ( 'NONE', #5932, #6035, #3093 ) ;
#16391 = ORIENTED_EDGE ( 'NONE', *, *, #5819, .T. ) ;
#16392 = VECTOR ( 'NONE', #1618, 1000.000000000000000 ) ;
#16393 = DIRECTION ( 'NONE',  ( 0.000000000000000000, 0.000000000000000000, 1.000000000000000000 ) ) ;
#16394 = AXIS2_PLACEMENT_3D ( 'NONE', #12949, #8567, #17342 ) ;
#16395 = ORIENTED_EDGE ( 'NONE', *, *, #1376, .T. ) ;
#16396 = AXIS2_PLACEMENT_3D ( 'NONE', #4203, #12869, #18668 ) ;
#16397 = FACE_OUTER_BOUND ( 'NONE', #6610, .T. ) ;
#16398 = CARTESIAN_POINT ( 'NONE',  ( 10.00000000000000000, 0.000000000000000000, 0.000000000000000000 ) ) ;
#16399 = DIRECTION ( 'NONE',  ( 0.9995004958639132076, 0.000000000000000000, 0.03160314490350067673 ) ) ;
#16400 = DIRECTION ( 'NONE',  ( -1.000000000000000000, 0.000000000000000000, 0.000000000000000000 ) ) ;
#16401 = CARTESIAN_POINT ( 'NONE',  ( 10.00000000000000000, 26.71881558261730660, 49.49802920186232313 ) ) ;
#16402 = ORIENTED_EDGE ( 'NONE', *, *, #18411, .F. ) ;
#16403 = DIRECTION ( 'NONE',  ( 0.000000000000000000, 0.000000000000000000, 1.000000000000000000 ) ) ;
#16404 = ORIENTED_EDGE ( 'NONE', *, *, #9995, .F. ) ;
#16405 = EDGE_CURVE ( 'NONE', #16237, #8582, #5303, .T. ) ;
#16406 = FILL_AREA_STYLE ('',( #3162 ) ) ;
#16407 = DIRECTION ( 'NONE',  ( -1.000000000000000000, 0.000000000000000000, 0.000000000000000000 ) ) ;
#16408 = ORIENTED_EDGE ( 'NONE', *, *, #10391, .F. ) ;
#16409 = CIRCLE ( 'NONE', #11229, 63.00000000006298961 ) ;
#16410 = EDGE_CURVE ( 'NONE', #3613, #11347, #2083, .T. ) ;
#16411 = ORIENTED_EDGE ( 'NONE', *, *, #16270, .T. ) ;
#16412 = EDGE_LOOP ( 'NONE', ( #2315, #8115, #6758, #5999 ) ) ;
#16413 = VERTEX_POINT ( 'NONE', #3610 ) ;
#16414 = CARTESIAN_POINT ( 'NONE',  ( 0.4999999999999916733, -30.39588787977742257, -2.000000000000000000 ) ) ;
#16415 = CIRCLE ( 'NONE', #14591, 5.000000000000004441 ) ;
#16416 = DIRECTION ( 'NONE',  ( 0.000000000000000000, -0.8910065241883722287, 0.4539904997395383668 ) ) ;
#16417 = CARTESIAN_POINT ( 'NONE',  ( 6.080745460913608902, 0.5192545390863916310, -1.000000000000000000 ) ) ;
#16418 = VECTOR ( 'NONE', #18114, 1000.000000000000000 ) ;
#16419 = CARTESIAN_POINT ( 'NONE',  ( -290.0000000000001137, -34.99999999999999289, -125.0000000000000000 ) ) ;
#16420 = CARTESIAN_POINT ( 'NONE',  ( 10.00000000000000000, -20.32630374611172641, -16.60877409751190470 ) ) ;
#16421 = CARTESIAN_POINT ( 'NONE',  ( 0.000000000000000000, 0.000000000000000000, 0.000000000000000000 ) ) ;
#16422 = ORIENTED_EDGE ( 'NONE', *, *, #7387, .T. ) ;
#16423 = CYLINDRICAL_SURFACE ( 'NONE', #18514, 25.00000000000000000 ) ;
#16424 = ORIENTED_EDGE ( 'NONE', *, *, #7362, .F. ) ;
#16425 = DIRECTION ( 'NONE',  ( 0.000000000000000000, 1.000000000000000000, 0.000000000000000000 ) ) ;
#16426 = DIRECTION ( 'NONE',  ( 0.000000000000000000, 0.1564344650402243464, 0.9876883405951388806 ) ) ;
#16427 = DIRECTION ( 'NONE',  ( -1.000000000000000000, -0.000000000000000000, -0.000000000000000000 ) ) ;
#16428 = VERTEX_POINT ( 'NONE', #6457 ) ;
#16429 = ORIENTED_EDGE ( 'NONE', *, *, #14347, .T. ) ;
#16430 = DIRECTION ( 'NONE',  ( -0.000000000000000000, 1.000000000000000000, -0.000000000000000000 ) ) ;
#16431 = CARTESIAN_POINT ( 'NONE',  ( -117.1020693116508085, -25.00000000000000000, 19.69080595179778115 ) ) ;
#16432 = DIRECTION ( 'NONE',  ( 0.000000000000000000, 0.4539904997395479147, -0.8910065241883673437 ) ) ;
#16433 = ORIENTED_EDGE ( 'NONE', *, *, #17266, .T. ) ;
#16434 = AXIS2_PLACEMENT_3D ( 'NONE', #10052, #11668, #15865 ) ;
#16435 = CIRCLE ( 'NONE', #15523, 56.24900000005625600 ) ;
#16436 = DIRECTION ( 'NONE',  ( -1.000000000000000000, -0.000000000000000000, -0.000000000000000000 ) ) ;
#16437 = DIRECTION ( 'NONE',  ( -1.000000000000000000, -0.000000000000000000, -0.000000000000000000 ) ) ;
#16438 = LINE ( 'NONE', #3389, #6310 ) ;
#16439 = ORIENTED_EDGE ( 'NONE', *, *, #10895, .T. ) ;
#16440 = EDGE_CURVE ( 'NONE', #16450, #5831, #13539, .T. ) ;
#16441 = DIRECTION ( 'NONE',  ( 0.000000000000000000, 0.000000000000000000, 1.000000000000000000 ) ) ;
#16442 = EDGE_CURVE ( 'NONE', #4722, #8684, #16262, .T. ) ;
#16443 = ORIENTED_EDGE ( 'NONE', *, *, #17483, .F. ) ;
#16444 = CYLINDRICAL_SURFACE ( 'NONE', #4205, 2.649999999999992806 ) ;
#16445 = VERTEX_POINT ( 'NONE', #16841 ) ;
#16446=STYLED_ITEM('',(#18890),#9701);
#16447 = DIRECTION ( 'NONE',  ( 0.000000000000000000, -0.1564344650402171299, -0.9876883405951398798 ) ) ;
#16448 = DIRECTION ( 'NONE',  ( 1.000000000000000000, 0.000000000000000000, 0.000000000000000000 ) ) ;
#16449 = ORIENTED_EDGE ( 'NONE', *, *, #686, .T. ) ;
#16450 = VERTEX_POINT ( 'NONE', #3789 ) ;
#16451 = CARTESIAN_POINT ( 'NONE',  ( -26.29305231718568336, -26.50000000000000000, -21.75302069950551953 ) ) ;
#16452 = ADVANCED_FACE ( 'NONE', ( #946 ), #12352, .T. ) ;
#16453 = ORIENTED_EDGE ( 'NONE', *, *, #9841, .F. ) ;
#16454 = DIRECTION ( 'NONE',  ( 1.000000000000000000, 0.000000000000000000, 0.000000000000000000 ) ) ;
#16455 = EDGE_CURVE ( 'NONE', #12567, #10719, #7779, .T. ) ;
#16456 = AXIS2_PLACEMENT_3D ( 'NONE', #2917, #8723, #2637 ) ;
#16457 = CARTESIAN_POINT ( 'NONE',  ( 4.141042297810615835, -2.227970268150433863, -3.687027686973623819 ) ) ;
#16458 = ORIENTED_EDGE ( 'NONE', *, *, #17395, .T. ) ;
#16459 = EDGE_CURVE ( 'NONE', #1893, #10035, #14736, .T. ) ;
#16460 = EDGE_CURVE ( 'NONE', #7904, #18365, #9254, .T. ) ;
#16461 = ORIENTED_EDGE ( 'NONE', *, *, #9246, .T. ) ;
#16462 = FACE_OUTER_BOUND ( 'NONE', #14326, .T. ) ;
#16463 = CARTESIAN_POINT ( 'NONE',  ( 0.000000000000000000, 42.79754323328179311, -13.90576474687299680 ) ) ;
#16464 = CARTESIAN_POINT ( 'NONE',  ( 0.000000000000000000, 14.19907017806900207, -22.07705612348824076 ) ) ;
#16465 = ORIENTED_EDGE ( 'NONE', *, *, #12632, .T. ) ;
#16466 = LINE ( 'NONE', #3419, #17272 ) ;
#16467 = ADVANCED_FACE ( 'NONE', ( #10821 ), #15408, .T. ) ;
#16468 = DIRECTION ( 'NONE',  ( -1.000000000000000000, -0.000000000000000000, -0.000000000000000000 ) ) ;
#16469 = DIRECTION ( 'NONE',  ( -0.000000000000000000, 1.000000000000000000, -0.000000000000000000 ) ) ;
#16470 = CARTESIAN_POINT ( 'NONE',  ( -1.654252653721913102, -3.663718938583024443, -0.01223254789874440342 ) ) ;
#16471 = VERTEX_POINT ( 'NONE', #12262 ) ;
#16472 = DIRECTION ( 'NONE',  ( 0.000000000000000000, 0.8090169943749486725, -0.5877852522924714718 ) ) ;
#16473 = EDGE_CURVE ( 'NONE', #276, #15649, #13611, .T. ) ;
#16474 = VECTOR ( 'NONE', #7580, 1000.000000000000000 ) ;
#16475 = LINE ( 'NONE', #9220, #10537 ) ;
#16476 = VERTEX_POINT ( 'NONE', #13881 ) ;
#16477 = DIRECTION ( 'NONE',  ( -1.000000000000000000, 0.000000000000000000, 0.000000000000000000 ) ) ;
#16478 = DIRECTION ( 'NONE',  ( 0.000000000000000000, -1.000000000000000000, 0.000000000000000000 ) ) ;
#16479 = AXIS2_PLACEMENT_3D ( 'NONE', #121, #1454, #12892 ) ;
#16480 = AXIS2_PLACEMENT_3D ( 'NONE', #863, #6666, #11232 ) ;
#16481 = ORIENTED_EDGE ( 'NONE', *, *, #4802, .F. ) ;
#16482 = CARTESIAN_POINT ( 'NONE',  ( 0.000000000000000000, -53.92768374110879392, -16.45250512421912603 ) ) ;
#16483 = ORIENTED_EDGE ( 'NONE', *, *, #1777, .F. ) ;
#16484 = CARTESIAN_POINT ( 'NONE',  ( -6.080745460913608902, 0.5192545390863924082, 0.000000000000000000 ) ) ;
#16485 = DIRECTION ( 'NONE',  ( 0.000000000000000000, -1.000000000000000000, 0.000000000000000000 ) ) ;
#16486 = AXIS2_PLACEMENT_3D ( 'NONE', #1612, #7414, #3140 ) ;
#16487 = CARTESIAN_POINT ( 'NONE',  ( 10.00000000000000000, 0.000000000000000000, 0.000000000000000000 ) ) ;
#16488 = CARTESIAN_POINT ( 'NONE',  ( 4.999999999999999112, -5.876895005581972420, -62.72529079327814117 ) ) ;
#16489 = DIRECTION ( 'NONE',  ( -0.000000000000000000, 1.000000000000000000, -0.000000000000000000 ) ) ;
#16490 = VERTEX_POINT ( 'NONE', #558 ) ;
#16491 = CARTESIAN_POINT ( 'NONE',  ( -79.64793068852927149, -30.00000000000000000, 29.21039329588766265 ) ) ;
#16492 = EDGE_CURVE ( 'NONE', #5638, #10659, #18084, .T. ) ;
#16493 =( NAMED_UNIT ( * ) PLANE_ANGLE_UNIT ( ) SI_UNIT ( $, .RADIAN. ) );
#16494 = CARTESIAN_POINT ( 'NONE',  ( -4.197393957002303999, -7.773935952363655451E-14, -3.503767560748929810 ) ) ;
#16495 = VERTEX_POINT ( 'NONE', #9408 ) ;
#16496 = ORIENTED_EDGE ( 'NONE', *, *, #395, .F. ) ;
#16497 = EDGE_LOOP ( 'NONE', ( #4627, #4183 ) ) ;
#16498 = ORIENTED_EDGE ( 'NONE', *, *, #8625, .T. ) ;
#16499 = CARTESIAN_POINT ( 'NONE',  ( 50.00005079999999680, 0.000000000000000000, 0.000000000000000000 ) ) ;
#16500 = FACE_OUTER_BOUND ( 'NONE', #5859, .T. ) ;
#16501 = DIRECTION ( 'NONE',  ( 0.000000000000000000, 1.000000000000000000, 0.000000000000000000 ) ) ;
#16502 = DIRECTION ( 'NONE',  ( -1.000000000000000000, 0.000000000000000000, -0.000000000000000000 ) ) ;
#16503 = CARTESIAN_POINT ( 'NONE',  ( 10.00000000000000000, 0.000000000000000000, 0.000000000000000000 ) ) ;
#16504 = DIRECTION ( 'NONE',  ( 0.000000000000000000, 0.000000000000000000, 1.000000000000000000 ) ) ;
#16505 = FACE_OUTER_BOUND ( 'NONE', #9410, .T. ) ;
#16506 = CARTESIAN_POINT ( 'NONE',  ( 5.000000000000000000, 32.70783759231086663, -4.381479206523104963 ) ) ;
#16507 = ORIENTED_EDGE ( 'NONE', *, *, #7143, .F. ) ;
#16508 = DIRECTION ( 'NONE',  ( 1.000000000000000000, -0.000000000000000000, -0.000000000000000000 ) ) ;
#16509 = VERTEX_POINT ( 'NONE', #750 ) ;
#16510 = EDGE_CURVE ( 'NONE', #24, #262, #1663, .T. ) ;
#16511 = AXIS2_PLACEMENT_3D ( 'NONE', #10437, #16628, #3593 ) ;
#16512 = DIRECTION ( 'NONE',  ( -1.000000000000000000, -0.000000000000000000, 0.000000000000000000 ) ) ;
#16513 = DIRECTION ( 'NONE',  ( -1.000000000000000000, -0.000000000000000000, 0.000000000000000000 ) ) ;
#16514 = AXIS2_PLACEMENT_3D ( 'NONE', #7558, #12408, #6789 ) ;
#16515 = DIRECTION ( 'NONE',  ( -1.000000000000000000, 0.000000000000000000, 0.000000000000000000 ) ) ;
#16516 = ORIENTED_EDGE ( 'NONE', *, *, #4369, .F. ) ;
#16517 = VERTEX_POINT ( 'NONE', #10329 ) ;
#16518 = AXIS2_PLACEMENT_3D ( 'NONE', #5905, #1895, #9038 ) ;
#16519 = CYLINDRICAL_SURFACE ( 'NONE', #8108, 24.00000000002400213 ) ;
#16520 = CARTESIAN_POINT ( 'NONE',  ( -26.29305231718568336, -21.50000000000000000, -19.10302069950552095 ) ) ;
#16521 = DIRECTION ( 'NONE',  ( 0.9938152567191714803, 0.000000000000000000, -0.1110460963393456596 ) ) ;
#16522 = ORIENTED_EDGE ( 'NONE', *, *, #13681, .T. ) ;
#16523 = PRODUCT_DEFINITION_SHAPE ( 'NONE', 'NONE',  #18810 ) ;
#16524 = ADVANCED_FACE ( 'NONE', ( #6827 ), #17043, .T. ) ;
#16525 = VECTOR ( 'NONE', #17570, 1000.000000000000000 ) ;
#16526 = CYLINDRICAL_SURFACE ( 'NONE', #9603, 24.00000000002399858 ) ;
#16527 = CARTESIAN_POINT ( 'NONE',  ( -290.0000000000001137, -34.99999999999999289, -125.0000000000000000 ) ) ;
#16528 = FACE_OUTER_BOUND ( 'NONE', #620, .T. ) ;
#16529 = ORIENTED_EDGE ( 'NONE', *, *, #14547, .T. ) ;
#16530 = DIRECTION ( 'NONE',  ( -1.000000000000000000, -0.000000000000000000, -0.000000000000000000 ) ) ;
#16531 = ADVANCED_FACE ( 'NONE', ( #11307 ), #14165, .F. ) ;
#16532 = ORIENTED_EDGE ( 'NONE', *, *, #4131, .T. ) ;
#16533 = CARTESIAN_POINT ( 'NONE',  ( -0.5000000000000000000, -30.39588787977742257, -2.000000000000000000 ) ) ;
#16534 = EDGE_LOOP ( 'NONE', ( #12996, #17853, #8094, #12454 ) ) ;
#16535 = CYLINDRICAL_SURFACE ( 'NONE', #14794, 10.00000000000000888 ) ;
#16536 = CARTESIAN_POINT ( 'NONE',  ( -1.243802165048909503, 3.900692638707381921, -3.223146290109805800 ) ) ;
#16537 = EDGE_LOOP ( 'NONE', ( #5602, #12847, #1479, #18332, #18089 ) ) ;
#16538 = ORIENTED_EDGE ( 'NONE', *, *, #10869, .F. ) ;
#16539 = CARTESIAN_POINT ( 'NONE',  ( 10.00000000000000000, -56.37237871411034718, 1.017308535512174261 ) ) ;
#16540 = ORIENTED_EDGE ( 'NONE', *, *, #17825, .T. ) ;
#16541 = CARTESIAN_POINT ( 'NONE',  ( 2.500000000000000000, -2.357898499370431722, 2.818925648462311528E-15 ) ) ;
#16542 = EDGE_CURVE ( 'NONE', #1960, #9593, #5628, .T. ) ;
#16543 = DIRECTION ( 'NONE',  ( 1.000000000000000000, -0.000000000000000000, 0.000000000000000000 ) ) ;
#16544 = VERTEX_POINT ( 'NONE', #3092 ) ;
#16545 = VERTEX_POINT ( 'NONE', #8801 ) ;
#16546 = DIRECTION ( 'NONE',  ( -1.000000000000000000, 0.000000000000000000, 0.000000000000000000 ) ) ;
#16547 = EDGE_CURVE ( 'NONE', #3360, #16545, #1010, .T. ) ;
#16548 = DIRECTION ( 'NONE',  ( 0.000000000000000000, 0.000000000000000000, 1.000000000000000000 ) ) ;
#16549 = DIRECTION ( 'NONE',  ( 1.000000000000000000, 0.000000000000000000, 0.000000000000000000 ) ) ;
#16550 = ORIENTED_EDGE ( 'NONE', *, *, #17599, .T. ) ;
#16551 = DIRECTION ( 'NONE',  ( -0.000000000000000000, 1.000000000000000000, -0.000000000000000000 ) ) ;
#16552 = CARTESIAN_POINT ( 'NONE',  ( -56.50000000009000445, -30.00000000000000000, 3.817814120399276590E-13 ) ) ;
#16553 = FACE_BOUND ( 'NONE', #13986, .T. ) ;
#16554 = CARTESIAN_POINT ( 'NONE',  ( 129.9999999999999432, -30.00000000000000000, -125.0000000000000000 ) ) ;
#16555 = ORIENTED_EDGE ( 'NONE', *, *, #4185, .T. ) ;
#16556 = CARTESIAN_POINT ( 'NONE',  ( 0.000000000000000000, -47.29147401531926675, -41.62350880771970196 ) ) ;
#16557 = EDGE_LOOP ( 'NONE', ( #9584, #12742 ) ) ;
#16558 = DIRECTION ( 'NONE',  ( -1.000000000000000000, 0.000000000000000000, 0.000000000000000000 ) ) ;
#16559 = DIRECTION ( 'NONE',  ( 0.000000000000000000, 0.000000000000000000, 1.000000000000000000 ) ) ;
#16560 =( REPRESENTATION_RELATIONSHIP ('NONE','NONE', #11014, #2517 ) REPRESENTATION_RELATIONSHIP_WITH_TRANSFORMATION ( #12682 )SHAPE_REPRESENTATION_RELATIONSHIP( ) );
#16561 = EDGE_CURVE ( 'NONE', #6386, #13569, #15907, .T. ) ;
#16562 = EDGE_CURVE ( 'NONE', #14980, #5515, #3437, .T. ) ;
#16563 =( GEOMETRIC_REPRESENTATION_CONTEXT ( 3 ) GLOBAL_UNCERTAINTY_ASSIGNED_CONTEXT ( ( #9765 ) ) GLOBAL_UNIT_ASSIGNED_CONTEXT ( ( #8832, #13412, #1595 ) ) REPRESENTATION_CONTEXT ( 'NONE', 'WORKASPACE' ) );
#16564 = ADVANCED_FACE ( 'NONE', ( #5508 ), #6033, .T. ) ;
#16565 = EDGE_CURVE ( 'NONE', #3234, #7366, #15612, .T. ) ;
#16566 = EDGE_LOOP ( 'NONE', ( #5459, #12112, #15581, #9187 ) ) ;
#16567 = EDGE_CURVE ( 'NONE', #12492, #7515, #5931, .T. ) ;
#16568 = EDGE_LOOP ( 'NONE', ( #15440, #11798, #12274, #18497 ) ) ;
#16569 = DIRECTION ( 'NONE',  ( 0.1305261922200517399, 0.9914448613738104932, 0.000000000000000000 ) ) ;
#16570 = LINE ( 'NONE', #10754, #2949 ) ;
#16571 = DIRECTION ( 'NONE',  ( -1.000000000000000000, -0.000000000000000000, -0.000000000000000000 ) ) ;
#16572 = EDGE_CURVE ( 'NONE', #16274, #15320, #14072, .T. ) ;
#16573 =( GEOMETRIC_REPRESENTATION_CONTEXT ( 3 ) GLOBAL_UNCERTAINTY_ASSIGNED_CONTEXT ( ( #7104 ) ) GLOBAL_UNIT_ASSIGNED_CONTEXT ( ( #11384, #9677, #14061 ) ) REPRESENTATION_CONTEXT ( 'NONE', 'WORKASPACE' ) );
#16574 = DIRECTION ( 'NONE',  ( -1.000000000000000000, 0.000000000000000000, 0.000000000000000000 ) ) ;
#16575 = AXIS2_PLACEMENT_3D ( 'NONE', #2912, #8720, #344 ) ;
#16576 = DIRECTION ( 'NONE',  ( 0.01644736842105263414, 0.9998647328874152862, -0.000000000000000000 ) ) ;
#16577 = VERTEX_POINT ( 'NONE', #6935 ) ;
#16578 = CARTESIAN_POINT ( 'NONE',  ( 10.04305231718579705, -26.50000000000000000, 30.90933677959249337 ) ) ;
#16579 = AXIS2_PLACEMENT_3D ( 'NONE', #12699, #11455, #3947 ) ;
#16580 = CARTESIAN_POINT ( 'NONE',  ( 10.00000000000000000, 24.33982105418971642, -50.71018745830419050 ) ) ;
#16581 = ORIENTED_EDGE ( 'NONE', *, *, #7021, .T. ) ;
#16582 = ADVANCED_FACE ( 'NONE', ( #17467 ), #7364, .T. ) ;
#16583 = ITEM_DEFINED_TRANSFORMATION ( 'NONE', 'NONE', #5316,  #8017 ) ;
#16584 = ORIENTED_EDGE ( 'NONE', *, *, #12858, .F. ) ;
#16585 = CIRCLE ( 'NONE', #6552, 12.00000000001200462 ) ;
#16586 = CARTESIAN_POINT ( 'NONE',  ( 10.00000000000000000, 0.000000000000000000, 0.000000000000000000 ) ) ;
#16587 = VERTEX_POINT ( 'NONE', #11217 ) ;
#16588 = AXIS2_PLACEMENT_3D ( 'NONE', #2593, #10120, #17090 ) ;
#16589 = EDGE_CURVE ( 'NONE', #16829, #17686, #3986, .T. ) ;
#16590 = VERTEX_POINT ( 'NONE', #8357 ) ;
#16591 = CARTESIAN_POINT ( 'NONE',  ( 10.00000000000000000, 0.000000000000000000, 26.24900000002624978 ) ) ;
#16592 = FILL_AREA_STYLE ('',( #1837 ) ) ;
#16593 = CARTESIAN_POINT ( 'NONE',  ( 0.000000000000000000, 3.000000000000000000, 0.000000000000000000 ) ) ;
#16594 = DIRECTION ( 'NONE',  ( 0.000000000000000000, 0.000000000000000000, 1.000000000000000000 ) ) ;
#16595 = DIRECTION ( 'NONE',  ( 1.000000000000000000, 0.000000000000000000, -0.000000000000000000 ) ) ;
#16596 = LINE ( 'NONE', #6316, #11337 ) ;
#16597 = VECTOR ( 'NONE', #18718, 1000.000000000000000 ) ;
#16598 = CYLINDRICAL_SURFACE ( 'NONE', #6243, 24.00000000002400213 ) ;
#16599 = ORIENTED_EDGE ( 'NONE', *, *, #10895, .F. ) ;
#16600 = DIRECTION ( 'NONE',  ( 0.000000000000000000, 0.000000000000000000, 1.000000000000000000 ) ) ;
#16601 = AXIS2_PLACEMENT_3D ( 'NONE', #15669, #14248, #7006 ) ;
#16602 = EDGE_LOOP ( 'NONE', ( #1410, #16758, #6955 ) ) ;
#16603 = CARTESIAN_POINT ( 'NONE',  ( 10.00000000000000000, 16.10733642026559309, -53.89344778774794520 ) ) ;
#16604 = CYLINDRICAL_SURFACE ( 'NONE', #9530, 4.799999999999999822 ) ;
#16605 = FACE_OUTER_BOUND ( 'NONE', #8353, .T. ) ;
#16606 = VERTEX_POINT ( 'NONE', #4415 ) ;
#16607 = AXIS2_PLACEMENT_3D ( 'NONE', #18416, #5375, #15570 ) ;
#16608 = ORIENTED_EDGE ( 'NONE', *, *, #13908, .F. ) ;
#16609 = CIRCLE ( 'NONE', #3802, 12.00000000001200640 ) ;
#16610 = DIRECTION ( 'NONE',  ( -1.000000000000000000, -0.000000000000000000, -0.000000000000000000 ) ) ;
#16611 = DIRECTION ( 'NONE',  ( 6.123233995736766036E-17, -1.000000000000000000, 0.000000000000000000 ) ) ;
#16612 = DIRECTION ( 'NONE',  ( -1.000000000000000000, -0.000000000000000000, -0.000000000000000000 ) ) ;
#16613 = ORIENTED_EDGE ( 'NONE', *, *, #8434, .F. ) ;
#16614 = CIRCLE ( 'NONE', #18750, 24.00000000002399858 ) ;
#16615 = AXIS2_PLACEMENT_3D ( 'NONE', #16383, #3514, #10833 ) ;
#16616 = EDGE_CURVE ( 'NONE', #12191, #1507, #7988, .T. ) ;
#16617 = DIRECTION ( 'NONE',  ( 0.000000000000000000, 0.000000000000000000, 1.000000000000000000 ) ) ;
#16618 = DIRECTION ( 'NONE',  ( 0.000000000000000000, 0.000000000000000000, 1.000000000000000000 ) ) ;
#16619 = CIRCLE ( 'NONE', #10828, 12.00000000001200640 ) ;
#16620 = AXIS2_PLACEMENT_3D ( 'NONE', #10996, #16733, #6526 ) ;
#16621 = CYLINDRICAL_SURFACE ( 'NONE', #17276, 55.00000000000000000 ) ;
#16622 = ORIENTED_EDGE ( 'NONE', *, *, #6025, .F. ) ;
#16623 = CARTESIAN_POINT ( 'NONE',  ( 2.500000000000000000, 1.178949249685218081, 2.041999999999998483 ) ) ;
#16624 = ORIENTED_EDGE ( 'NONE', *, *, #6437, .T. ) ;
#16625 = CARTESIAN_POINT ( 'NONE',  ( 10.00000000000000000, 0.000000000000000000, 0.000000000000000000 ) ) ;
#16626 = VERTEX_POINT ( 'NONE', #9876 ) ;
#16627 = CARTESIAN_POINT ( 'NONE',  ( 1.828356344711641102, 3.563200125723180900, -5.433716356636336675E-16 ) ) ;
#16628 = DIRECTION ( 'NONE',  ( -0.000000000000000000, 1.000000000000000000, -0.000000000000000000 ) ) ;
#16629 = AXIS2_PLACEMENT_3D ( 'NONE', #7778, #9125, #7408 ) ;
#16630 = EDGE_LOOP ( 'NONE', ( #17892, #8689 ) ) ;
#16631 = VERTEX_POINT ( 'NONE', #12840 ) ;
#16632 = CIRCLE ( 'NONE', #14759, 56.24900000005627021 ) ;
#16633 = CARTESIAN_POINT ( 'NONE',  ( 0.000000000000000000, -20.41355805489602204, -19.44239304137396118 ) ) ;
#16634 = AXIS2_PLACEMENT_3D ( 'NONE', #7808, #13631, #15247 ) ;
#16635 = EDGE_CURVE ( 'NONE', #13520, #16959, #5248, .T. ) ;
#16636 = ORIENTED_EDGE ( 'NONE', *, *, #8024, .T. ) ;
#16637 = LINE ( 'NONE', #10638, #14292 ) ;
#16638 = AXIS2_PLACEMENT_3D ( 'NONE', #5908, #742, #7526 ) ;
#16639 = AXIS2_PLACEMENT_3D ( 'NONE', #10847, #10946, #6388 ) ;
#16640 = EDGE_CURVE ( 'NONE', #10166, #4084, #16043, .T. ) ;
#16641 = CARTESIAN_POINT ( 'NONE',  ( 10.00000000000000000, 0.000000000000000000, 0.000000000000000000 ) ) ;
#16642 = VECTOR ( 'NONE', #18504, 1000.000000000000000 ) ;
#16643 = DIRECTION ( 'NONE',  ( 0.000000000000000000, 0.000000000000000000, 1.000000000000000000 ) ) ;
#16644 = VERTEX_POINT ( 'NONE', #13657 ) ;
#16645 = CIRCLE ( 'NONE', #846, 2.649999999999992806 ) ;
#16646 = VECTOR ( 'NONE', #13757, 1000.000000000000000 ) ;
#16647 = CIRCLE ( 'NONE', #7523, 2.649999999999985700 ) ;
#16648 = VECTOR ( 'NONE', #6893, 1000.000000000000000 ) ;
#16649 = ORIENTED_EDGE ( 'NONE', *, *, #14529, .T. ) ;
#16650 = CARTESIAN_POINT ( 'NONE',  ( 4.235886605889389145, 2.417314728048528760, -3.751161874094018245 ) ) ;
#16651 = CIRCLE ( 'NONE', #15132, 63.00000000006298961 ) ;
#16652 = CARTESIAN_POINT ( 'NONE',  ( 0.000000000000000000, 33.71303790549275448, 53.22058882792209289 ) ) ;
#16653 = DIRECTION ( 'NONE',  ( -1.000000000000000000, 0.000000000000000000, 0.000000000000000000 ) ) ;
#16654 = EDGE_LOOP ( 'NONE', ( #4841, #2909, #10088, #8747 ) ) ;
#16655 = DIRECTION ( 'NONE',  ( -0.000000000000000000, 1.000000000000000000, -0.000000000000000000 ) ) ;
#16656 = LINE ( 'NONE', #14078, #4527 ) ;
#16657 = DIRECTION ( 'NONE',  ( 0.000000000000000000, 0.000000000000000000, 1.000000000000000000 ) ) ;
#16658 = CARTESIAN_POINT ( 'NONE',  ( -11.25000000000000355, 0.000000000000000000, 25.10000000000000142 ) ) ;
#16659 = EDGE_LOOP ( 'NONE', ( #8727, #15780, #6519, #15850, #2731, #17458 ) ) ;
#16660 = CARTESIAN_POINT ( 'NONE',  ( -0.3562533529037968383, 13.24999999999999467, 23.49729949480461499 ) ) ;
#16661 = ORIENTED_EDGE ( 'NONE', *, *, #11665, .T. ) ;
#16662 = CARTESIAN_POINT ( 'NONE',  ( -4.211140560182196957, -2.431303136016552013, -3.745885042887436178 ) ) ;
#16663 = CARTESIAN_POINT ( 'NONE',  ( -1.200950573245989306, 11.24999999999999645, 24.97113769375797432 ) ) ;
#16664 = CIRCLE ( 'NONE', #7528, 12.00000000001200462 ) ;
#16665 = CIRCLE ( 'NONE', #18804, 24.00000000002400213 ) ;
#16666 = AXIS2_PLACEMENT_3D ( 'NONE', #7002, #14242, #10135 ) ;
#16667 = CIRCLE ( 'NONE', #5104, 63.00000000006298961 ) ;
#16668 = ORIENTED_EDGE ( 'NONE', *, *, #8714, .F. ) ;
#16669 = CIRCLE ( 'NONE', #248, 41.00000000000000000 ) ;
#16670 = ORIENTED_EDGE ( 'NONE', *, *, #13897, .F. ) ;
#16671 = DIRECTION ( 'NONE',  ( 0.000000000000000000, 1.000000000000000000, 0.000000000000000000 ) ) ;
#16672 = PLANE ( 'NONE',  #11823 ) ;
#16673 = DIRECTION ( 'NONE',  ( -1.000000000000000000, -0.000000000000000000, 0.000000000000000000 ) ) ;
#16674 = FACE_OUTER_BOUND ( 'NONE', #11881, .T. ) ;
#16675 = EDGE_CURVE ( 'NONE', #15108, #17376, #10775, .T. ) ;
#16676 = AXIS2_PLACEMENT_3D ( 'NONE', #9844, #1368, #18513 ) ;
#16677 = EDGE_CURVE ( 'NONE', #4773, #15536, #11653, .T. ) ;
#16678 = FACE_OUTER_BOUND ( 'NONE', #8564, .T. ) ;
#16679 = AXIS2_PLACEMENT_3D ( 'NONE', #12692, #14110, #18502 ) ;
#16680 = DIRECTION ( 'NONE',  ( 0.000000000000000000, 0.000000000000000000, -1.000000000000000000 ) ) ;
#16681 = ORIENTED_EDGE ( 'NONE', *, *, #13606, .T. ) ;
#16682 = CIRCLE ( 'NONE', #2693, 33.00000000003299760 ) ;
#16683 = CARTESIAN_POINT ( 'NONE',  ( -90.00000000009001155, 1.000000000000014655, -1.301042606982603940E-15 ) ) ;
#16684 = APPLICATION_CONTEXT ( 'automotive_design' ) ;
#16685 = EDGE_CURVE ( 'NONE', #18250, #8867, #384, .T. ) ;
#16686 = PRESENTATION_STYLE_ASSIGNMENT (( #15804 ) ) ;
#16687 = CARTESIAN_POINT ( 'NONE',  ( -4.000000000000000000, -0.7890432684750890990, -0.04868663549882315533 ) ) ;
#16688 = ORIENTED_EDGE ( 'NONE', *, *, #18566, .T. ) ;
#16689 = EDGE_CURVE ( 'NONE', #10808, #4800, #7370, .T. ) ;
#16690 = ORIENTED_EDGE ( 'NONE', *, *, #615, .T. ) ;
#16691 = CIRCLE ( 'NONE', #3617, 0.09999999999999939493 ) ;
#16692 = VECTOR ( 'NONE', #15237, 1000.000000000000000 ) ;
#16693 = VERTEX_POINT ( 'NONE', #16420 ) ;
#16694 = ADVANCED_FACE ( 'NONE', ( #16505 ), #6126, .F. ) ;
#16695 = AXIS2_PLACEMENT_3D ( 'NONE', #17914, #14874, #14675 ) ;
#16696 = VECTOR ( 'NONE', #3794, 1000.000000000000000 ) ;
#16697 = ORIENTED_EDGE ( 'NONE', *, *, #11323, .T. ) ;
#16698 = DIRECTION ( 'NONE',  ( 0.000000000000000000, -1.000000000000000000, 1.287488025362403787E-15 ) ) ;
#16699 = CARTESIAN_POINT ( 'NONE',  ( 10.00000000000000000, -19.44239304137360946, -20.41355805489636310 ) ) ;
#16700 = DIRECTION ( 'NONE',  ( 1.000000000000000000, 0.000000000000000000, 0.000000000000000000 ) ) ;
#16701 = CARTESIAN_POINT ( 'NONE',  ( -117.1020693116506379, -38.00000000000000000, -19.69080595179801207 ) ) ;
#16702 = EDGE_CURVE ( 'NONE', #17432, #13289, #16596, .T. ) ;
#16703 = CARTESIAN_POINT ( 'NONE',  ( -79.64793068852898728, -30.00000000000000000, -31.86039329588756530 ) ) ;
#16704 = EDGE_CURVE ( 'NONE', #12626, #7339, #4694, .T. ) ;
#16705 = DIRECTION ( 'NONE',  ( -0.000000000000000000, 1.000000000000000000, -0.000000000000000000 ) ) ;
#16706 = CIRCLE ( 'NONE', #10316, 5.000000000000004441 ) ;
#16707 = DIRECTION ( 'NONE',  ( 0.000000000000000000, -0.9510565162951500895, -0.3090169943749581649 ) ) ;
#16708 = DIRECTION ( 'NONE',  ( 0.9914448613738102711, -0.1305261922200524338, 0.000000000000000000 ) ) ;
#16709 = ORIENTED_EDGE ( 'NONE', *, *, #7147, .F. ) ;
#16710 = DIRECTION ( 'NONE',  ( 0.000000000000000000, 0.000000000000000000, 1.000000000000000000 ) ) ;
#16711 = ORIENTED_EDGE ( 'NONE', *, *, #14641, .F. ) ;
#16712 = CIRCLE ( 'NONE', #1202, 24.00000000002399858 ) ;
#16713 = EDGE_CURVE ( 'NONE', #7504, #944, #14383, .T. ) ;
#16714 = CARTESIAN_POINT ( 'NONE',  ( -2.595115354961444076, -7.673029147243174641, -1.000000000000000000 ) ) ;
#16715 = CARTESIAN_POINT ( 'NONE',  ( 10.00000000000000000, -62.72529079327802748, -5.876895005583096854 ) ) ;
#16716 = ORIENTED_EDGE ( 'NONE', *, *, #11280, .F. ) ;
#16717 = ORIENTED_EDGE ( 'NONE', *, *, #11567, .F. ) ;
#16718 = ADVANCED_FACE ( 'NONE', ( #4971 ), #12123, .T. ) ;
#16719 = DIRECTION ( 'NONE',  ( -1.000000000000000000, -0.000000000000000000, -0.000000000000000000 ) ) ;
#16720 = DIRECTION ( 'NONE',  ( 1.892183365217058947E-17, -1.000000000000000000, 5.823541592445467890E-17 ) ) ;
#16721 = CARTESIAN_POINT ( 'NONE',  ( 0.000000000000000000, -12.18267823974769293, 25.42247726998010648 ) ) ;
#16722 = VERTEX_POINT ( 'NONE', #17745 ) ;
#16723 = CIRCLE ( 'NONE', #8503, 5.384454397937118664 ) ;
#16724 = AXIS2_PLACEMENT_3D ( 'NONE', #16503, #13936, #2410 ) ;
#16725 = DIRECTION ( 'NONE',  ( -1.000000000000000000, 0.000000000000000000, 0.000000000000000000 ) ) ;
#16726 = DIRECTION ( 'NONE',  ( 0.000000000000000000, -0.000000000000000000, 1.000000000000000000 ) ) ;
#16727 = CARTESIAN_POINT ( 'NONE',  ( 10.00000000000000000, 29.03656532225586062, -15.68049343255964523 ) ) ;
#16728 = ORIENTED_EDGE ( 'NONE', *, *, #8024, .F. ) ;
#16729 = DIRECTION ( 'NONE',  ( -1.000000000000000000, -0.000000000000000000, -0.000000000000000000 ) ) ;
#16730 = ORIENTED_EDGE ( 'NONE', *, *, #5547, .F. ) ;
#16731 = LINE ( 'NONE', #18049, #18188 ) ;
#16732 = ORIENTED_EDGE ( 'NONE', *, *, #12052, .T. ) ;
#16733 = DIRECTION ( 'NONE',  ( -1.000000000000000000, -0.000000000000000000, -0.000000000000000000 ) ) ;
#16734 = DIRECTION ( 'NONE',  ( -0.000000000000000000, -0.000000000000000000, -1.000000000000000000 ) ) ;
#16735 = CIRCLE ( 'NONE', #8515, 12.00000000001200462 ) ;
#16736 = VERTEX_POINT ( 'NONE', #13380 ) ;
#16737 = ORIENTED_EDGE ( 'NONE', *, *, #767, .F. ) ;
#16738 = EDGE_CURVE ( 'NONE', #16785, #2490, #16200, .T. ) ;
#16739 = DIRECTION ( 'NONE',  ( -1.000000000000000000, 0.000000000000000000, 0.000000000000000000 ) ) ;
#16740 = VERTEX_POINT ( 'NONE', #7732 ) ;
#16741 = DIRECTION ( 'NONE',  ( -1.000000000000000000, -0.000000000000000000, -0.000000000000000000 ) ) ;
#16742 = SHAPE_REPRESENTATION ( 'stationary ring', ( #8017 ), #737 ) ;
#16743 = DIRECTION ( 'NONE',  ( 0.000000000000000000, -0.5877852522924624790, -0.8090169943749551118 ) ) ;
#16744 = DIRECTION ( 'NONE',  ( 0.000000000000000000, 0.000000000000000000, -1.000000000000000000 ) ) ;
#16745 = ORIENTED_EDGE ( 'NONE', *, *, #15426, .T. ) ;
#16746 = ADVANCED_FACE ( 'NONE', ( #11847 ), #3465, .F. ) ;
#16747 = VERTEX_POINT ( 'NONE', #10498 ) ;
#16748 = CYLINDRICAL_SURFACE ( 'NONE', #17279, 2.649999999999999467 ) ;
#16749 = DIRECTION ( 'NONE',  ( 0.000000000000000000, 1.000000000000000000, 0.000000000000000000 ) ) ;
#16750 = CARTESIAN_POINT ( 'NONE',  ( 10.00000000000000000, -19.44239304137360946, -20.41355805489636310 ) ) ;
#16751 = ORIENTED_EDGE ( 'NONE', *, *, #8424, .T. ) ;
#16752 = FACE_OUTER_BOUND ( 'NONE', #5305, .T. ) ;
#16753 = EDGE_LOOP ( 'NONE', ( #13537, #7725, #16076, #4541 ) ) ;
#16754 = EDGE_CURVE ( 'NONE', #5801, #6887, #3562, .T. ) ;
#16755 = CARTESIAN_POINT ( 'NONE',  ( 10.04305231718605285, -26.50000000000000000, -30.90933677959240811 ) ) ;
#16756 = CYLINDRICAL_SURFACE ( 'NONE', #11333, 63.00000000006298961 ) ;
#16757 = ORIENTED_EDGE ( 'NONE', *, *, #7596, .T. ) ;
#16758 = ORIENTED_EDGE ( 'NONE', *, *, #17728, .T. ) ;
#16759 = CARTESIAN_POINT ( 'NONE',  ( 10.00000000000000000, 19.44239304137375868, 20.41355805489622455 ) ) ;
#16760 = ORIENTED_EDGE ( 'NONE', *, *, #18573, .T. ) ;
#16761 = FACE_OUTER_BOUND ( 'NONE', #14343, .T. ) ;
#16762 = DIRECTION ( 'NONE',  ( -1.000000000000000000, 0.000000000000000000, -0.000000000000000000 ) ) ;
#16763 =( GEOMETRIC_REPRESENTATION_CONTEXT ( 3 ) GLOBAL_UNCERTAINTY_ASSIGNED_CONTEXT ( ( #9191 ) ) GLOBAL_UNIT_ASSIGNED_CONTEXT ( ( #8172, #14270, #5406 ) ) REPRESENTATION_CONTEXT ( 'NONE', 'WORKASPACE' ) );
#16764 = B_SPLINE_CURVE_WITH_KNOTS ( 'NONE', 3,
 ( #16662, #18081, #5023, #1411, #4091, #11518 ),
 .UNSPECIFIED., .F., .F.,
 ( 4, 2, 4 ),
 ( -3.640115492409406142E-06, 0.0002066546034003385283, 0.0004169493222930864334 ),
 .UNSPECIFIED. ) ;
#16765 = SHAPE_REPRESENTATION ( 'socket head cap screw_iso_ISO 4762 M5 x 30 - 22N', ( #8017 ), #2572 ) ;
#16766 = EDGE_CURVE ( 'NONE', #17515, #18364, #15288, .T. ) ;
#16767 = EDGE_LOOP ( 'NONE', ( #12305, #4159, #10110, #9454, #4140 ) ) ;
#16768 = ADVANCED_FACE ( 'NONE', ( #3276 ), #13559, .F. ) ;
#16769 = EDGE_LOOP ( 'NONE', ( #15087, #801, #16939, #11937 ) ) ;
#16770 = CARTESIAN_POINT ( 'NONE',  ( 0.000000000000000000, -53.22058882792220658, 33.71303790549256263 ) ) ;
#16771 = CARTESIAN_POINT ( 'NONE',  ( 129.9999999999999432, -34.99999999999999289, -125.0000000000000000 ) ) ;
#16772 = CYLINDRICAL_SURFACE ( 'NONE', #18157, 2.649999999999992806 ) ;
#16773 = CARTESIAN_POINT ( 'NONE',  ( 0.000000000000000000, -55.83748330407413363, 7.813799127873079620 ) ) ;
#16774 = AXIS2_PLACEMENT_3D ( 'NONE', #10432, #73, #16345 ) ;
#16775 = EDGE_CURVE ( 'NONE', #4499, #1486, #11028, .T. ) ;
#16776 = DIRECTION ( 'NONE',  ( 0.000000000000000000, 0.000000000000000000, -1.000000000000000000 ) ) ;
#16777 = CARTESIAN_POINT ( 'NONE',  ( 5.000000000000000000, -47.29147401531984229, 41.62350880771904826 ) ) ;
#16778 = ORIENTED_EDGE ( 'NONE', *, *, #3069, .T. ) ;
#16779 = DIRECTION ( 'NONE',  ( -1.000000000000000000, -0.000000000000000000, -0.000000000000000000 ) ) ;
#16780 = CARTESIAN_POINT ( 'NONE',  ( -2.595115354961444076, -7.673029147243174641, 0.000000000000000000 ) ) ;
#16781 = ORIENTED_EDGE ( 'NONE', *, *, #7270, .T. ) ;
#16782 = ORIENTED_EDGE ( 'NONE', *, *, #15356, .T. ) ;
#16783 = ADVANCED_FACE ( 'NONE', ( #9258, #3178, #14791 ), #1745, .F. ) ;
#16784 = EDGE_CURVE ( 'NONE', #6, #2422, #11940, .T. ) ;
#16785 = VERTEX_POINT ( 'NONE', #5467 ) ;
#16786 = VERTEX_POINT ( 'NONE', #2413 ) ;
#16788 = CARTESIAN_POINT ( 'NONE',  ( 10.00000000000000000, 56.37237871411034007, 25.01730853553658207 ) ) ;
#16787 = CIRCLE ( 'NONE', #16172, 30.39999999999999858 ) ;
#16789 = DIRECTION ( 'NONE',  ( 0.000000000000000000, 0.000000000000000000, 1.000000000000000000 ) ) ;
#16790 = DIRECTION ( 'NONE',  ( 0.000000000000000000, 0.000000000000000000, -1.000000000000000000 ) ) ;
#16791 = CARTESIAN_POINT ( 'NONE',  ( 0.000000000000000000, -32.11449294037157642, -54.20017844242546090 ) ) ;
#16792 = DIRECTION ( 'NONE',  ( 1.000000000000000000, 0.000000000000000000, 0.000000000000000000 ) ) ;
#16793 = LINE ( 'NONE', #2304, #10995 ) ;
#16794 = DIRECTION ( 'NONE',  ( -1.000000000000000000, -0.000000000000000000, 0.000000000000000000 ) ) ;
#16795 = ORIENTED_EDGE ( 'NONE', *, *, #7218, .T. ) ;
#16796 = CARTESIAN_POINT ( 'NONE',  ( 10.00000000000000000, 0.000000000000000000, 0.000000000000000000 ) ) ;
#16797 = ORIENTED_EDGE ( 'NONE', *, *, #6335, .F. ) ;
#16798 = FACE_OUTER_BOUND ( 'NONE', #15151, .T. ) ;
#16799 = DIRECTION ( 'NONE',  ( 1.000000000000000000, 0.000000000000000000, 0.000000000000000000 ) ) ;
#16800 = EDGE_LOOP ( 'NONE', ( #15072, #17156, #13738, #9111 ) ) ;
#16801 = VERTEX_POINT ( 'NONE', #8123 ) ;
#16802 = CARTESIAN_POINT ( 'NONE',  ( -10.00000000000000000, 0.000000000000000000, 0.000000000000000000 ) ) ;
#16803 = DIRECTION ( 'NONE',  ( 1.000000000000000000, 6.123233995736766036E-17, -6.123233995736764803E-17 ) ) ;
#16804 = VECTOR ( 'NONE', #4204, 1000.000000000000000 ) ;
#16805 = DIRECTION ( 'NONE',  ( 0.000000000000000000, 1.000000000000000000, 3.491481338843133355E-15 ) ) ;
#16806 = ORIENTED_EDGE ( 'NONE', *, *, #10265, .F. ) ;
#16807 = EDGE_CURVE ( 'NONE', #16626, #8925, #2523, .T. ) ;
#16808 = EDGE_CURVE ( 'NONE', #6735, #1940, #9512, .T. ) ;
#16809 = EDGE_CURVE ( 'NONE', #12910, #13484, #9813, .T. ) ;
#16810 = CARTESIAN_POINT ( 'NONE',  ( -10.00000000000000000, 0.000000000000000000, 0.000000000000000000 ) ) ;
#16811 = EDGE_CURVE ( 'NONE', #16644, #2861, #18032, .T. ) ;
#16812 = DIRECTION ( 'NONE',  ( 0.000000000000000000, 0.000000000000000000, 1.000000000000000000 ) ) ;
#16813 = DIRECTION ( 'NONE',  ( -1.000000000000000000, 0.000000000000000000, 0.000000000000000000 ) ) ;
#16814 = ORIENTED_EDGE ( 'NONE', *, *, #12564, .T. ) ;
#16815 = CARTESIAN_POINT ( 'NONE',  ( 3.999999999999999112, -1.539600717839012978, -3.300726591567080703 ) ) ;
#16816 = CIRCLE ( 'NONE', #8292, 2.649999999999999467 ) ;
#16817 = CIRCLE ( 'NONE', #8604, 56.24900000005625600 ) ;
#16818 = ORIENTED_EDGE ( 'NONE', *, *, #9457, .T. ) ;
#16819 = DIRECTION ( 'NONE',  ( 0.000000000000000000, 0.000000000000000000, 1.000000000000000000 ) ) ;
#16820 = ORIENTED_EDGE ( 'NONE', *, *, #12039, .T. ) ;
#16821 = APPLICATION_CONTEXT ( 'automotive_design' ) ;
#16822 = EDGE_CURVE ( 'NONE', #10550, #6419, #102, .T. ) ;
#16823 = CARTESIAN_POINT ( 'NONE',  ( 1.654252653721905331, 3.663718938583014229, -0.01223254789873410957 ) ) ;
#16824 = CARTESIAN_POINT ( 'NONE',  ( 0.000000000000000000, 0.000000000000000000, 0.000000000000000000 ) ) ;
#16825 = DIRECTION ( 'NONE',  ( 0.000000000000000000, -0.7071067811865535679, 0.7071067811865413555 ) ) ;
#16826 = ORIENTED_EDGE ( 'NONE', *, *, #16713, .F. ) ;
#16827 = ORIENTED_EDGE ( 'NONE', *, *, #15124, .T. ) ;
#16828 = CARTESIAN_POINT ( 'NONE',  ( 27.29487558977753991, 1.305124410222461284, 0.000000000000000000 ) ) ;
#16829 = VERTEX_POINT ( 'NONE', #8319 ) ;
#16830 = DIRECTION ( 'NONE',  ( -1.000000000000000000, 0.000000000000000000, -0.000000000000000000 ) ) ;
#16831 = EDGE_CURVE ( 'NONE', #18403, #14393, #10970, .T. ) ;
#16832 = CIRCLE ( 'NONE', #2842, 2.649999999999999467 ) ;
#16833 = AXIS2_PLACEMENT_3D ( 'NONE', #12087, #5024, #17903 ) ;
#16834 = FACE_OUTER_BOUND ( 'NONE', #6231, .T. ) ;
#16835 = DIRECTION ( 'NONE',  ( 0.000000000000000000, -1.000000000000000000, 0.000000000000000000 ) ) ;
#16836 = EDGE_CURVE ( 'NONE', #9267, #13789, #990, .T. ) ;
#16837 = ORIENTED_EDGE ( 'NONE', *, *, #11900, .F. ) ;
#16838 = DIRECTION ( 'NONE',  ( 0.000000000000000000, 0.000000000000000000, -1.000000000000000000 ) ) ;
#16839 = VERTEX_POINT ( 'NONE', #8228 ) ;
#16840 = CARTESIAN_POINT ( 'NONE',  ( -0.1756481739660520902, 4.720212674038980261, -3.469390959564065291 ) ) ;
#16841 = CARTESIAN_POINT ( 'NONE',  ( -0.9999999999999986677, -27.60846790388774608, 0.000000000000000000 ) ) ;
#16842 = FACE_OUTER_BOUND ( 'NONE', #14702, .T. ) ;
#16843 = ORIENTED_EDGE ( 'NONE', *, *, #10405, .T. ) ;
#16844 = DIRECTION ( 'NONE',  ( 1.000000000000000000, 0.000000000000000000, 0.000000000000000000 ) ) ;
#16845 = ORIENTED_EDGE ( 'NONE', *, *, #11249, .T. ) ;
#16846 = VECTOR ( 'NONE', #17094, 1000.000000000000000 ) ;
#16847 = DIRECTION ( 'NONE',  ( -0.000000000000000000, 1.000000000000000000, -0.000000000000000000 ) ) ;
#16848 = CARTESIAN_POINT ( 'NONE',  ( 10.00000000000000000, 0.000000000000000000, 0.000000000000000000 ) ) ;
#16849 = ORIENTED_EDGE ( 'NONE', *, *, #8890, .T. ) ;
#16850 = ORIENTED_EDGE ( 'NONE', *, *, #17985, .F. ) ;
#16851 =( LENGTH_UNIT ( ) NAMED_UNIT ( * ) SI_UNIT ( .MILLI., .METRE. ) );
#16852 = ORIENTED_EDGE ( 'NONE', *, *, #13871, .T. ) ;
#16853 = CARTESIAN_POINT ( 'NONE',  ( -17.77999999999999758, 3.061616997868383043E-15, -25.00000000000000000 ) ) ;
#16854 = DIRECTION ( 'NONE',  ( -0.000000000000000000, -1.000000000000000000, -0.000000000000000000 ) ) ;
#16855 =( GEOMETRIC_REPRESENTATION_CONTEXT ( 3 ) GLOBAL_UNCERTAINTY_ASSIGNED_CONTEXT ( ( #826 ) ) GLOBAL_UNIT_ASSIGNED_CONTEXT ( ( #11317, #3539, #4088 ) ) REPRESENTATION_CONTEXT ( 'NONE', 'WORKASPACE' ) );
#16856 = EDGE_CURVE ( 'NONE', #17183, #17331, #13176, .T. ) ;
#16857 = VERTEX_POINT ( 'NONE', #9745 ) ;
#16858 = ORIENTED_EDGE ( 'NONE', *, *, #2759, .F. ) ;
#16859 = CARTESIAN_POINT ( 'NONE',  ( 0.000000000000000000, -46.20417134726153563, 32.31183295104756326 ) ) ;
#16860 = PLANE ( 'NONE',  #2402 ) ;
#16861 = DIRECTION ( 'NONE',  ( 1.000000000000000000, 0.000000000000000000, 0.000000000000000000 ) ) ;
#16862 = FACE_OUTER_BOUND ( 'NONE', #5138, .T. ) ;
#16863 = PLANE ( 'NONE',  #13347 ) ;
#16864 = DIRECTION ( 'NONE',  ( 0.000000000000000000, 0.000000000000000000, 1.000000000000000000 ) ) ;
#16865 = CARTESIAN_POINT ( 'NONE',  ( 4.211140560182196957, -2.431303136016555122, -3.745885042887436622 ) ) ;
#16866 = ORIENTED_EDGE ( 'NONE', *, *, #14885, .T. ) ;
#16867 = DIRECTION ( 'NONE',  ( 0.000000000000000000, 0.000000000000000000, 1.000000000000000000 ) ) ;
#16868 = MECHANICAL_DESIGN_GEOMETRIC_PRESENTATION_REPRESENTATION (  '', ( #14130 ), #16252 ) ;
#16869 = CARTESIAN_POINT ( 'NONE',  ( 10.00000000000000000, 1.335003989222417697, -56.23315539212688918 ) ) ;
#16870 = DIRECTION ( 'NONE',  ( -0.000000000000000000, 1.000000000000000000, -0.000000000000000000 ) ) ;
#16871 = EDGE_CURVE ( 'NONE', #5833, #14748, #16817, .T. ) ;
#16872 = CONTEXT_DEPENDENT_SHAPE_REPRESENTATION ( #14621, #3448 ) ;
#16873 = VERTEX_POINT ( 'NONE', #18116 ) ;
#16874 = EDGE_CURVE ( 'NONE', #11197, #1295, #16793, .T. ) ;
#16875 = VERTEX_POINT ( 'NONE', #6877 ) ;
#16876 = ORIENTED_EDGE ( 'NONE', *, *, #220, .T. ) ;
#16877 = AXIS2_PLACEMENT_3D ( 'NONE', #6423, #12227, #13755 ) ;
#16878 = CARTESIAN_POINT ( 'NONE',  ( 50.00005079999999680, 6.123233995736766282E-16, -5.000000000000000000 ) ) ;
#16879 = DIRECTION ( 'NONE',  ( 0.000000000000000000, 0.000000000000000000, 1.000000000000000000 ) ) ;
#16880 = AXIS2_PLACEMENT_3D ( 'NONE', #10544, #9205, #6073 ) ;
#16881 = CARTESIAN_POINT ( 'NONE',  ( 0.000000000000000000, 6.123233995736766282E-16, -5.000000000000000000 ) ) ;
#16882 = VECTOR ( 'NONE', #7887, 1000.000000000000000 ) ;
#16883 = DIRECTION ( 'NONE',  ( 1.000000000000000000, 0.000000000000000000, 0.000000000000000000 ) ) ;
#16884 = DIRECTION ( 'NONE',  ( 0.000000000000000000, 0.8090169943749485615, -0.5877852522924714718 ) ) ;
#16885 = CARTESIAN_POINT ( 'NONE',  ( 0.000000000000000000, -5.120903701083534543E-13, -42.35000000000000142 ) ) ;
#16886 = CYLINDRICAL_SURFACE ( 'NONE', #4915, 24.00000000002400213 ) ;
#16887 = DIRECTION ( 'NONE',  ( 0.000000000000000000, 0.000000000000000000, -1.000000000000000000 ) ) ;
#16888 = ORIENTED_EDGE ( 'NONE', *, *, #14864, .F. ) ;
#16889 = CARTESIAN_POINT ( 'NONE',  ( -10.00000000000000000, 0.000000000000000000, 0.000000000000000000 ) ) ;
#16890 = VERTEX_POINT ( 'NONE', #6701 ) ;
#16891 = DIRECTION ( 'NONE',  ( -1.000000000000000000, -0.000000000000000000, 0.000000000000000000 ) ) ;
#16892 = DIRECTION ( 'NONE',  ( 0.000000000000000000, 0.9510565162951523099, 0.3090169943749515036 ) ) ;
#16893 = ORIENTED_EDGE ( 'NONE', *, *, #12502, .T. ) ;
#16894 = ORIENTED_EDGE ( 'NONE', *, *, #12921, .T. ) ;
#16895 = DIRECTION ( 'NONE',  ( -1.000000000000000000, 0.000000000000000000, 0.000000000000000000 ) ) ;
#16896 = CARTESIAN_POINT ( 'NONE',  ( -36.40576474687286179, -14.99999999999999289, 26.45033635316097076 ) ) ;
#16897 = PRODUCT_DEFINITION_FORMATION_WITH_SPECIFIED_SOURCE ( 'ANY', '', #9377, .NOT_KNOWN. ) ;
#16898 = CARTESIAN_POINT ( 'NONE',  ( -90.00000000009003998, 1.000000000000018208, -5.746271514173173500E-15 ) ) ;
#16899 = ORIENTED_EDGE ( 'NONE', *, *, #644, .T. ) ;
#16900 = AXIS2_PLACEMENT_3D ( 'NONE', #12124, #2306, #13939 ) ;
#16901 = DIRECTION ( 'NONE',  ( 0.000000000000000000, 0.4539904997395412534, 0.8910065241883707854 ) ) ;
#16902 = CARTESIAN_POINT ( 'NONE',  ( 10.00000000000000000, 0.000000000000000000, 0.000000000000000000 ) ) ;
#16903 = CIRCLE ( 'NONE', #16301, 28.00000000000000355 ) ;
#16904 = CARTESIAN_POINT ( 'NONE',  ( 0.000000000000000000, 1.178949249685213863, -2.042000000000001148 ) ) ;
#16905 = CARTESIAN_POINT ( 'NONE',  ( 4.000000000000000000, -1.084202172485504434E-14, -3.142992957459231906 ) ) ;
#16906 = VECTOR ( 'NONE', #4346, 1000.000000000000000 ) ;
#16907 = ORIENTED_EDGE ( 'NONE', *, *, #9064, .T. ) ;
#16908 = DIRECTION ( 'NONE',  ( 0.000000000000000000, -1.000000000000000000, 0.000000000000000000 ) ) ;
#16909 = CIRCLE ( 'NONE', #13854, 56.24900000005625600 ) ;
#16910 = ORIENTED_EDGE ( 'NONE', *, *, #6119, .T. ) ;
#16911 = EDGE_CURVE ( 'NONE', #652, #11271, #9481, .T. ) ;
#16912 = EDGE_CURVE ( 'NONE', #18379, #24, #10390, .T. ) ;
#16913 = EDGE_CURVE ( 'NONE', #8709, #2515, #18612, .T. ) ;
#16914 = CARTESIAN_POINT ( 'NONE',  ( 5.000000000000000000, 14.27431201565524788, 29.75305054077477607 ) ) ;
#16915 = DIRECTION ( 'NONE',  ( 0.000000000000000000, 0.000000000000000000, -1.000000000000000000 ) ) ;
#16916 = DIRECTION ( 'NONE',  ( 0.000000000000000000, 0.3090169943749410120, 0.9510565162951556406 ) ) ;
#16917 = ORIENTED_EDGE ( 'NONE', *, *, #12978, .T. ) ;
#16918 = ORIENTED_EDGE ( 'NONE', *, *, #10036, .F. ) ;
#16919 = DIRECTION ( 'NONE',  ( 0.000000000000000000, -0.000000000000000000, 1.000000000000000000 ) ) ;
#16920 = EDGE_CURVE ( 'NONE', #3669, #6075, #13829, .T. ) ;
#16921 = VERTEX_POINT ( 'NONE', #8019 ) ;
#16922 = DIRECTION ( 'NONE',  ( 0.000000000000000000, 0.000000000000000000, 1.000000000000000000 ) ) ;
#16923 = AXIS2_PLACEMENT_3D ( 'NONE', #914, #16610, #2224 ) ;
#16924 = AXIS2_PLACEMENT_3D ( 'NONE', #56, #1380, #18622 ) ;
#16925 = AXIS2_PLACEMENT_3D ( 'NONE', #11729, #17719, #207 ) ;
#16926 = AXIS2_PLACEMENT_3D ( 'NONE', #14330, #15763, #12904 ) ;
#16927 = AXIS2_PLACEMENT_3D ( 'NONE', #5387, #2155, #7957 ) ;
#16928 = AXIS2_PLACEMENT_3D ( 'NONE', #678, #1255, #5618 ) ;
#16929 = DIRECTION ( 'NONE',  ( 0.000000000000000000, 0.000000000000000000, 1.000000000000000000 ) ) ;
#16930 = EDGE_CURVE ( 'NONE', #7123, #6555, #795, .T. ) ;
#16931 = CARTESIAN_POINT ( 'NONE',  ( -4.000000000000000000, -2.309401076758512694, -5.000000000000000000 ) ) ;
#16932 =( REPRESENTATION_RELATIONSHIP ('NONE','NONE', #11014, #2517 ) REPRESENTATION_RELATIONSHIP_WITH_TRANSFORMATION ( #8765 )SHAPE_REPRESENTATION_RELATIONSHIP( ) );
#16933 = ORIENTED_EDGE ( 'NONE', *, *, #8548, .T. ) ;
#16934 = DIRECTION ( 'NONE',  ( -1.000000000000000000, 0.000000000000000000, -0.000000000000000000 ) ) ;
#16935 = ORIENTED_EDGE ( 'NONE', *, *, #16640, .T. ) ;
#16936 = CARTESIAN_POINT ( 'NONE',  ( 3.472371940585993855, 2.614027278893175321, -3.320322319201766792 ) ) ;
#16937 = CARTESIAN_POINT ( 'NONE',  ( 10.00000000000000000, 0.000000000000000000, 0.000000000000000000 ) ) ;
#16938 = CARTESIAN_POINT ( 'NONE',  ( 0.000000000000000000, 25.38428207620322752, 6.681932690257054830 ) ) ;
#16939 = ORIENTED_EDGE ( 'NONE', *, *, #13544, .T. ) ;
#16940 = CARTESIAN_POINT ( 'NONE',  ( 0.000000000000000000, 0.000000000000000000, -2.000000000000000000 ) ) ;
#16942 = VERTEX_POINT ( 'NONE', #10309 ) ;
#16941 = ADVANCED_FACE ( 'NONE', ( #11059 ), #16886, .T. ) ;
#16943 = AXIS2_PLACEMENT_3D ( 'NONE', #16773, #17915, #9522 ) ;
#16944 = ADVANCED_FACE ( 'NONE', ( #16117 ), #2982, .F. ) ;
#16945 = DIRECTION ( 'NONE',  ( -1.000000000000000000, 0.000000000000000000, -0.000000000000000000 ) ) ;
#16946 = CYLINDRICAL_SURFACE ( 'NONE', #4345, 12.00000000001200462 ) ;
#16947 = AXIS2_PLACEMENT_3D ( 'NONE', #898, #3940, #18017 ) ;
#16948 = ORIENTED_EDGE ( 'NONE', *, *, #11490, .F. ) ;
#16949 = ORIENTED_EDGE ( 'NONE', *, *, #383, .F. ) ;
#16950 = AXIS2_PLACEMENT_3D ( 'NONE', #11531, #2766, #17067 ) ;
#16951 = VERTEX_POINT ( 'NONE', #17367 ) ;
#16952 = DIRECTION ( 'NONE',  ( -0.000000000000000000, 1.000000000000000000, -0.000000000000000000 ) ) ;
#16953 = CARTESIAN_POINT ( 'NONE',  ( 10.00000000000000000, 34.13306034420251223, -44.70888270294124567 ) ) ;
#16954 = ADVANCED_FACE ( 'NONE', ( #16018 ), #1876, .T. ) ;
#16955 = VECTOR ( 'NONE', #9880, 1000.000000000000000 ) ;
#16956 = VECTOR ( 'NONE', #14311, 1000.000000000000000 ) ;
#16957 = VECTOR ( 'NONE', #10774, 1000.000000000000000 ) ;
#16958 = ORIENTED_EDGE ( 'NONE', *, *, #7499, .F. ) ;
#16959 = VERTEX_POINT ( 'NONE', #8780 ) ;
#16960 = DIRECTION ( 'NONE',  ( 0.000000000000000000, 0.9876883405951371042, 0.1564344650402347547 ) ) ;
#16961 = CARTESIAN_POINT ( 'NONE',  ( 4.203935335434060505, 1.640780671294165272, -3.598452447879202598 ) ) ;
#16962 = DIRECTION ( 'NONE',  ( 0.000000000000000000, 0.000000000000000000, -1.000000000000000000 ) ) ;
#16963 = CARTESIAN_POINT ( 'NONE',  ( 10.00000000000000000, 0.000000000000000000, 0.000000000000000000 ) ) ;
#16964 = B_SPLINE_CURVE_WITH_KNOTS ( 'NONE', 3,
 ( #14608, #6027, #7359, #11841, #14510, #11747 ),
 .UNSPECIFIED., .F., .F.,
 ( 4, 2, 4 ),
 ( 0.000000000000000000, 0.0002095117440864783663, 0.0004190234881729567326 ),
 .UNSPECIFIED. ) ;
#16965 = LINE ( 'NONE', #14196, #1472 ) ;
#16966 = DIRECTION ( 'NONE',  ( -1.000000000000000000, 0.000000000000000000, 0.000000000000000000 ) ) ;
#16967 = CIRCLE ( 'NONE', #2058, 33.00000000003299760 ) ;
#16968 = CARTESIAN_POINT ( 'NONE',  ( -56.50000000009000445, -38.00000000000000000, 3.817814120399276590E-13 ) ) ;
#16969 = ORIENTED_EDGE ( 'NONE', *, *, #14850, .T. ) ;
#16970 = CARTESIAN_POINT ( 'NONE',  ( -0.5636800770129166693, -4.293361309317430319, -3.531542292955206275 ) ) ;
#16971 = CARTESIAN_POINT ( 'NONE',  ( 0.000000000000000000, 29.75305054077472633, 14.27431201565535979 ) ) ;
#16972 = AXIS2_PLACEMENT_3D ( 'NONE', #14038, #14123, #15268 ) ;
#16973 = DIRECTION ( 'NONE',  ( -0.000000000000000000, 1.103561164596346103E-15, 1.000000000000000000 ) ) ;
#16974 = DIRECTION ( 'NONE',  ( 1.000000000000000000, 0.000000000000000000, -0.000000000000000000 ) ) ;
#16975 = AXIS2_PLACEMENT_3D ( 'NONE', #11864, #1949, #9381 ) ;
#16976 = AXIS2_PLACEMENT_3D ( 'NONE', #1628, #18789, #3155 ) ;
#16977 = EDGE_CURVE ( 'NONE', #9630, #5675, #13446, .T. ) ;
#16978 = ITEM_DEFINED_TRANSFORMATION ( 'NONE', 'NONE', #4419,  #8017 ) ;
#16979 = VERTEX_POINT ( 'NONE', #2879 ) ;
#16980 = B_SPLINE_CURVE_WITH_KNOTS ( 'NONE', 3,
 ( #12668, #8478, #1155, #7044, #2669, #15718, #1337, #6957 ),
 .UNSPECIFIED., .F., .F.,
 ( 4, 2, 2, 4 ),
 ( 0.000000000000000000, 0.002450665683189818828, 0.003675998524784728459, 0.004901331366379638524 ),
 .UNSPECIFIED. ) ;
#16981 = ORIENTED_EDGE ( 'NONE', *, *, #7942, .T. ) ;
#16982 = VECTOR ( 'NONE', #17132, 1000.000000000000000 ) ;
#16983 = ORIENTED_EDGE ( 'NONE', *, *, #9650, .F. ) ;
#16984 = AXIS2_PLACEMENT_3D ( 'NONE', #13455, #9062, #3359 ) ;
#16985 = FACE_OUTER_BOUND ( 'NONE', #5564, .T. ) ;
#16986 =( LENGTH_UNIT ( ) NAMED_UNIT ( * ) SI_UNIT ( .MILLI., .METRE. ) );
#16987 = CIRCLE ( 'NONE', #16066, 1.249999999999999778 ) ;
#16988 = AXIS2_PLACEMENT_3D ( 'NONE', #17517, #7326, #5616 ) ;
#16989 = CARTESIAN_POINT ( 'NONE',  ( 0.000000000000000000, 0.000000000000000000, 0.000000000000000000 ) ) ;
#16990 = CARTESIAN_POINT ( 'NONE',  ( 0.000000000000000000, 45.00825343885021113, 33.95787273855260935 ) ) ;
#16991 = DIRECTION ( 'NONE',  ( 0.000000000000000000, 0.000000000000000000, 1.000000000000000000 ) ) ;
#16992 = EDGE_CURVE ( 'NONE', #3828, #1353, #6439, .T. ) ;
#16993 = LINE ( 'NONE', #3944, #11182 ) ;
#16994 = DIRECTION ( 'NONE',  ( 0.000000000000000000, 0.9510565162951545304, -0.3090169943749446202 ) ) ;
#16995 = DIRECTION ( 'NONE',  ( 0.000000000000000000, 1.000000000000000000, 3.491481338843133355E-15 ) ) ;
#16996 = ORIENTED_EDGE ( 'NONE', *, *, #4566, .F. ) ;
#16997 = LINE ( 'NONE', #15265, #11225 ) ;
#16998 = ORIENTED_EDGE ( 'NONE', *, *, #8194, .F. ) ;
#16999 = EDGE_CURVE ( 'NONE', #12362, #1018, #2485, .T. ) ;
#17000 = DIRECTION ( 'NONE',  ( 0.000000000000000000, -0.4999999999999989453, 0.8660254037844391517 ) ) ;
#17001 = CARTESIAN_POINT ( 'NONE',  ( -290.0000000000001137, -34.99999999999999289, -125.0000000000000000 ) ) ;
#17002 = VECTOR ( 'NONE', #14820, 1000.000000000000000 ) ;
#17003 = ORIENTED_EDGE ( 'NONE', *, *, #16992, .T. ) ;
#17004 = ORIENTED_EDGE ( 'NONE', *, *, #16836, .F. ) ;
#17005 = CARTESIAN_POINT ( 'NONE',  ( 10.00000000000000000, 55.83748330407408389, -7.813799127873475747 ) ) ;
#17006 = CARTESIAN_POINT ( 'NONE',  ( 10.04305231718605107, -39.99999999999999289, -30.90933677959241166 ) ) ;
#17007 = VECTOR ( 'NONE', #13238, 1000.000000000000000 ) ;
#17008 = DIRECTION ( 'NONE',  ( -1.000000000000000000, 0.000000000000000000, -0.000000000000000000 ) ) ;
#17009 = VERTEX_POINT ( 'NONE', #7344 ) ;
#17010 = PRESENTATION_LAYER_ASSIGNMENT (  '', '', ( #5445 ) ) ;
#17011 = AXIS2_PLACEMENT_3D ( 'NONE', #16755, #16847, #18074 ) ;
#17012 = DIRECTION ( 'NONE',  ( -1.000000000000000000, 0.000000000000000000, 0.000000000000000000 ) ) ;
#17013 = CARTESIAN_POINT ( 'NONE',  ( 2.500000000000000000, 1.768423874527823791, 1.020999999999998353 ) ) ;
#17014 = CIRCLE ( 'NONE', #17314, 12.00000000001200817 ) ;
#17015 = CARTESIAN_POINT ( 'NONE',  ( 0.000000000000000000, -14.27431201565505425, -29.75305054077487199 ) ) ;
#17016 = CARTESIAN_POINT ( 'NONE',  ( -10.00000000000000000, 0.000000000000000000, 0.000000000000000000 ) ) ;
#17017 = CIRCLE ( 'NONE', #1195, 63.00000000006298961 ) ;
#17018 = UNCERTAINTY_MEASURE_WITH_UNIT (LENGTH_MEASURE( 1.000000000000000082E-05 ), #2840, 'distance_accuracy_value', 'NONE');
#17019 = CIRCLE ( 'NONE', #14482, 5.000000000000004441 ) ;
#17020 = DIRECTION ( 'NONE',  ( 0.000000000000000000, 0.000000000000000000, 1.000000000000000000 ) ) ;
#17021 = ORIENTED_EDGE ( 'NONE', *, *, #10039, .F. ) ;
#17022 = DIRECTION ( 'NONE',  ( -1.000000000000000000, 0.000000000000000000, -0.000000000000000000 ) ) ;
#17023 = DIRECTION ( 'NONE',  ( -1.000000000000000000, -0.000000000000000000, -0.000000000000000000 ) ) ;
#17024 = DIRECTION ( 'NONE',  ( 0.000000000000000000, 0.000000000000000000, 1.000000000000000000 ) ) ;
#17025 = EDGE_LOOP ( 'NONE', ( #16411, #12595, #5516, #16424 ) ) ;
#17026 = ORIENTED_EDGE ( 'NONE', *, *, #10968, .F. ) ;
#17027 = CARTESIAN_POINT ( 'NONE',  ( 0.000000000000000000, -25.42247726998023083, 12.18267823974742470 ) ) ;
#17028 =( NAMED_UNIT ( * ) SI_UNIT ( $, .STERADIAN. ) SOLID_ANGLE_UNIT ( ) );
#17029 = EDGE_LOOP ( 'NONE', ( #9312, #4130, #6801, #15234 ) ) ;
#17030 = LINE ( 'NONE', #15781, #17934 ) ;
#17031 = AXIS2_PLACEMENT_3D ( 'NONE', #17726, #3255, #16403 ) ;
#17032 = AXIS2_PLACEMENT_3D ( 'NONE', #6820, #12631, #18436 ) ;
#17033 = EDGE_CURVE ( 'NONE', #10536, #3234, #12795, .T. ) ;
#17034 = DIRECTION ( 'NONE',  ( 0.000000000000000000, 0.9510565162951521989, 0.3090169943749515036 ) ) ;
#17035 = ADVANCED_FACE ( 'NONE', ( #5745 ), #7055, .F. ) ;
#17036 = CARTESIAN_POINT ( 'NONE',  ( 0.000000000000000000, 27.72801475327282361, 6.913036516934699449 ) ) ;
#17037 = EDGE_LOOP ( 'NONE', ( #11837, #3550, #10081, #3528 ) ) ;
#17038 = DIRECTION ( 'NONE',  ( -1.000000000000000000, -0.000000000000000000, 0.000000000000000000 ) ) ;
#17039 = AXIS2_PLACEMENT_3D ( 'NONE', #5540, #15823, #1163 ) ;
#17040 = ORIENTED_EDGE ( 'NONE', *, *, #3612, .T. ) ;
#17042 = CYLINDRICAL_SURFACE ( 'NONE', #9339, 26.24900000002624978 ) ;
#17041 = PRODUCT_DEFINITION_CONTEXT ( 'detailed design', #15708, 'design' ) ;
#17043 = CYLINDRICAL_SURFACE ( 'NONE', #8956, 0.7499999999999997780 ) ;
#17044 = DIRECTION ( 'NONE',  ( -1.000000000000000000, -0.000000000000000000, -0.000000000000000000 ) ) ;
#17045 = EDGE_LOOP ( 'NONE', ( #17643, #4460, #3212, #9240 ) ) ;
#17046 = DIRECTION ( 'NONE',  ( -1.000000000000000000, 0.000000000000000000, 0.000000000000000000 ) ) ;
#17047 = EDGE_LOOP ( 'NONE', ( #10251, #1866, #18781, #6810 ) ) ;
#17048 =( GEOMETRIC_REPRESENTATION_CONTEXT ( 3 ) GLOBAL_UNCERTAINTY_ASSIGNED_CONTEXT ( ( #2150 ) ) GLOBAL_UNIT_ASSIGNED_CONTEXT ( ( #3560, #15181, #9450 ) ) REPRESENTATION_CONTEXT ( 'NONE', 'WORKASPACE' ) );
#17049 = CYLINDRICAL_SURFACE ( 'NONE', #14266, 12.00000000001200462 ) ;
#17050 = CARTESIAN_POINT ( 'NONE',  ( 10.00000000000000000, -24.79895094899269026, 13.40641754777657013 ) ) ;
#17051 = ORIENTED_EDGE ( 'NONE', *, *, #1681, .T. ) ;
#17052 = ORIENTED_EDGE ( 'NONE', *, *, #10747, .F. ) ;
#17053 = FILL_AREA_STYLE_COLOUR ( '', #3556 ) ;
#17055 = ADVANCED_FACE ( 'NONE', ( #11731 ), #17275, .F. ) ;
#17054 = VERTEX_POINT ( 'NONE', #2696 ) ;
#17056 = FACE_OUTER_BOUND ( 'NONE', #3044, .T. ) ;
#17057 = CARTESIAN_POINT ( 'NONE',  ( 0.000000000000000000, 53.06836994729258805, -18.64666490672316712 ) ) ;
#17058 = AXIS2_PLACEMENT_3D ( 'NONE', #13468, #49, #5845 ) ;
#17059 = EDGE_CURVE ( 'NONE', #18246, #2561, #12983, .T. ) ;
#17060 = VECTOR ( 'NONE', #6309, 1000.000000000000000 ) ;
#17061 = EDGE_CURVE ( 'NONE', #17928, #16109, #14491, .T. ) ;
#17062 = ORIENTED_EDGE ( 'NONE', *, *, #14697, .T. ) ;
#17063 = EDGE_CURVE ( 'NONE', #5694, #7722, #17541, .T. ) ;
#17064 = ORIENTED_EDGE ( 'NONE', *, *, #8580, .F. ) ;
#17065 = CARTESIAN_POINT ( 'NONE',  ( 10.00000000000000000, 53.29895248911700634, -18.38754094778185788 ) ) ;
#17066 = DIRECTION ( 'NONE',  ( 0.000000000000000000, 0.000000000000000000, 1.000000000000000000 ) ) ;
#17068 = EDGE_CURVE ( 'NONE', #2784, #6911, #4225, .T. ) ;
#17067 = DIRECTION ( 'NONE',  ( 0.000000000000000000, 0.3090169943749480619, -0.9510565162951533091 ) ) ;
#17069 = DIRECTION ( 'NONE',  ( 0.000000000000000000, 0.000000000000000000, 1.000000000000000000 ) ) ;
#17070 = CYLINDRICAL_SURFACE ( 'NONE', #11818, 2.649999999999999467 ) ;
#17071 = CARTESIAN_POINT ( 'NONE',  ( 10.00000000000000000, -29.75305054077482225, 14.27431201565513597 ) ) ;
#17072 = LINE ( 'NONE', #4104, #3848 ) ;
#17073 = VERTEX_POINT ( 'NONE', #15839 ) ;
#17074 = CARTESIAN_POINT ( 'NONE',  ( -1.274258131565027874, -3.883108878240886241, -3.220599429844051009 ) ) ;
#17075 = VECTOR ( 'NONE', #5592, 1000.000000000000000 ) ;
#17076 = DIRECTION ( 'NONE',  ( 0.000000000000000000, 0.000000000000000000, 1.000000000000000000 ) ) ;
#17077 = ADVANCED_FACE ( 'NONE', ( #7157 ), #4397, .F. ) ;
#17078 = CARTESIAN_POINT ( 'NONE',  ( -90.00000000009001155, -13.00000000000001776, -1.691355389077386325E-15 ) ) ;
#17079 = CARTESIAN_POINT ( 'NONE',  ( 0.000000000000000000, -30.00000000000000000, 20.00000000000000000 ) ) ;
#17080 = VERTEX_POINT ( 'NONE', #10027 ) ;
#17081 = ORIENTED_EDGE ( 'NONE', *, *, #6751, .F. ) ;
#17082 = ORIENTED_EDGE ( 'NONE', *, *, #5281, .F. ) ;
#17083 = DIRECTION ( 'NONE',  ( 0.000000000000000000, 1.000000000000000000, 0.000000000000000000 ) ) ;
#17084 = CARTESIAN_POINT ( 'NONE',  ( 10.00000000000000000, 0.000000000000000000, 0.000000000000000000 ) ) ;
#17085 = ADVANCED_FACE ( 'NONE', ( #15744 ), #12520, .F. ) ;
#17086 = CARTESIAN_POINT ( 'NONE',  ( 4.000000000000000000, 0.7924765000094659007, -0.05906175389889852662 ) ) ;
#17087 = DIRECTION ( 'NONE',  ( -1.000000000000000000, -0.000000000000000000, -0.000000000000000000 ) ) ;
#17088 = CARTESIAN_POINT ( 'NONE',  ( -90.00000000009001155, -34.99999999999999289, -1.301042606982603940E-15 ) ) ;
#17089 = DIRECTION ( 'NONE',  ( 0.000000000000000000, 0.000000000000000000, 1.000000000000000000 ) ) ;
#17090 = DIRECTION ( 'NONE',  ( 0.000000000000000000, 0.000000000000000000, 1.000000000000000000 ) ) ;
#17091 = EDGE_LOOP ( 'NONE', ( #13925, #5130 ) ) ;
#17092 = DIRECTION ( 'NONE',  ( 1.000000000000000000, 0.000000000000000000, 0.000000000000000000 ) ) ;
#17093 = ORIENTED_EDGE ( 'NONE', *, *, #5572, .F. ) ;
#17094 = DIRECTION ( 'NONE',  ( 2.031314180040284764E-16, 1.000000000000000000, 1.301042606982601377E-16 ) ) ;
#17095 = CARTESIAN_POINT ( 'NONE',  ( 0.000000000000000000, -16.10733642026522006, 53.89344778774805889 ) ) ;
#17096 = ORIENTED_EDGE ( 'NONE', *, *, #7990, .T. ) ;
#17097 = CARTESIAN_POINT ( 'NONE',  ( -94.77031323234206184, 1.000000000000018208, 0.5330212624288539480 ) ) ;
#17098 = CIRCLE ( 'NONE', #965, 26.24900000002625333 ) ;
#17099 = DIRECTION ( 'NONE',  ( 1.000000000000000000, 6.123233995736766036E-17, -6.123233995736764803E-17 ) ) ;
#17100 = DIRECTION ( 'NONE',  ( 1.000000000000000000, 0.000000000000000000, 0.000000000000000000 ) ) ;
#17101 = ORIENTED_EDGE ( 'NONE', *, *, #7942, .F. ) ;
#17102 = VECTOR ( 'NONE', #3156, 1000.000000000000000 ) ;
#17103 = FACE_BOUND ( 'NONE', #1029, .T. ) ;
#17104 = CARTESIAN_POINT ( 'NONE',  ( 5.000000000000000000, 41.62350880771986539, -47.29147401531912465 ) ) ;
#17105 = CARTESIAN_POINT ( 'NONE',  ( 0.000000000000000000, 0.000000000000000000, 0.000000000000000000 ) ) ;
#17106 = EDGE_CURVE ( 'NONE', #11928, #17219, #4313, .T. ) ;
#17107 = CARTESIAN_POINT ( 'NONE',  ( 0.000000000000000000, -13.75000000000000533, 25.00000000000000000 ) ) ;
#17108 = FACE_OUTER_BOUND ( 'NONE', #5301, .T. ) ;
#17109 = VERTEX_POINT ( 'NONE', #9148 ) ;
#17110 = AXIS2_PLACEMENT_3D ( 'NONE', #8933, #11889, #17347 ) ;
#17111 = CARTESIAN_POINT ( 'NONE',  ( 10.00000000000000000, 0.000000000000000000, 0.000000000000000000 ) ) ;
#17112 = CARTESIAN_POINT ( 'NONE',  ( 10.00000000000000000, -49.76630880786327538, 26.49895292617986797 ) ) ;
#17113 = DIRECTION ( 'NONE',  ( 0.000000000000000000, 0.000000000000000000, 1.000000000000000000 ) ) ;
#17114 = ORIENTED_EDGE ( 'NONE', *, *, #14255, .F. ) ;
#17115 = ORIENTED_EDGE ( 'NONE', *, *, #3883, .T. ) ;
#17116 = DIRECTION ( 'NONE',  ( 0.000000000000000000, 0.000000000000000000, 1.000000000000000000 ) ) ;
#17117 = FILL_AREA_STYLE ('',( #2728 ) ) ;
#17118 = ORIENTED_EDGE ( 'NONE', *, *, #15067, .F. ) ;
#17119 = LINE ( 'NONE', #14344, #9714 ) ;
#17120 = EDGE_CURVE ( 'NONE', #7406, #12720, #4675, .T. ) ;
#17121 = PRODUCT_DEFINITION_SHAPE ( 'NONE', 'NONE',  #15630 ) ;
#17122 = ADVANCED_FACE ( 'NONE', ( #14968 ), #13358, .T. ) ;
#17123 = VECTOR ( 'NONE', #9982, 1000.000000000000000 ) ;
#17124 = CARTESIAN_POINT ( 'NONE',  ( 2.500000000000000000, 0.000000000000000000, 0.000000000000000000 ) ) ;
#17125 = AXIS2_PLACEMENT_3D ( 'NONE', #12746, #17131, #4077 ) ;
#17126 = DIRECTION ( 'NONE',  ( 1.000000000000000000, 0.000000000000000000, 0.000000000000000000 ) ) ;
#17127 = EDGE_LOOP ( 'NONE', ( #1405, #15658, #4006, #18244 ) ) ;
#17128 = DIRECTION ( 'NONE',  ( -0.000000000000000000, 0.000000000000000000, -1.000000000000000000 ) ) ;
#17129 = VERTEX_POINT ( 'NONE', #4865 ) ;
#17130 = LINE ( 'NONE', #1645, #2969 ) ;
#17131 = DIRECTION ( 'NONE',  ( -0.000000000000000000, 1.000000000000000000, -0.000000000000000000 ) ) ;
#17132 = DIRECTION ( 'NONE',  ( -1.000000000000000000, 0.000000000000000000, 0.000000000000000000 ) ) ;
#17133 = ORIENTED_EDGE ( 'NONE', *, *, #1170, .F. ) ;
#17134 = DIRECTION ( 'NONE',  ( 0.000000000000000000, -1.000000000000000000, 0.000000000000000000 ) ) ;
#17135 = ORIENTED_EDGE ( 'NONE', *, *, #12500, .T. ) ;
#17136 = DIRECTION ( 'NONE',  ( 0.000000000000000000, 0.000000000000000000, 1.000000000000000000 ) ) ;
#17137 = DIRECTION ( 'NONE',  ( -0.000000000000000000, -0.000000000000000000, -1.000000000000000000 ) ) ;
#17138 = EDGE_LOOP ( 'NONE', ( #13208, #6953, #4955 ) ) ;
#17139 = VERTEX_POINT ( 'NONE', #209 ) ;
#17140 = DIRECTION ( 'NONE',  ( 0.000000000000000000, 0.000000000000000000, 1.000000000000000000 ) ) ;
#17141 = CIRCLE ( 'NONE', #4057, 63.00000000006298961 ) ;
#17142 = ORIENTED_EDGE ( 'NONE', *, *, #14839, .F. ) ;
#17143 = CARTESIAN_POINT ( 'NONE',  ( 0.000000000000000000, 0.000000000000000000, 1.500000000000000000 ) ) ;
#17144 = CARTESIAN_POINT ( 'NONE',  ( -117.1020693116506379, -30.00000000000000000, -17.04080595179801705 ) ) ;
#17145 = CIRCLE ( 'NONE', #13177, 24.00000000002399858 ) ;
#17146 = ORIENTED_EDGE ( 'NONE', *, *, #7016, .T. ) ;
#17147 = CIRCLE ( 'NONE', #12266, 2.649999999999999467 ) ;
#17148 = ORIENTED_EDGE ( 'NONE', *, *, #15067, .T. ) ;
#17149 = CARTESIAN_POINT ( 'NONE',  ( 10.00000000000000000, 39.14194549634421350, -40.58063702438301590 ) ) ;
#17150 = DIRECTION ( 'NONE',  ( -1.000000000000000000, -0.000000000000000000, -0.000000000000000000 ) ) ;
#17151 = DIRECTION ( 'NONE',  ( 0.000000000000000000, 0.4539904997395412534, 0.8910065241883707854 ) ) ;
#17152 = DIRECTION ( 'NONE',  ( -0.000000000000000000, -0.000000000000000000, -1.000000000000000000 ) ) ;
#17153 = DIRECTION ( 'NONE',  ( 0.000000000000000000, 0.000000000000000000, -1.000000000000000000 ) ) ;
#17154 = DIRECTION ( 'NONE',  ( 0.000000000000000000, 0.000000000000000000, 1.000000000000000000 ) ) ;
#17155 = DIRECTION ( 'NONE',  ( 0.000000000000000000, 0.000000000000000000, 1.000000000000000000 ) ) ;
#17156 = ORIENTED_EDGE ( 'NONE', *, *, #16616, .F. ) ;
#17157 = CYLINDRICAL_SURFACE ( 'NONE', #17039, 23.50000000000001066 ) ;
#17158 = EDGE_CURVE ( 'NONE', #12191, #3837, #7711, .T. ) ;
#17159 = EDGE_CURVE ( 'NONE', #14286, #7462, #16787, .T. ) ;
#17160 = DIRECTION ( 'NONE',  ( -1.000000000000000000, 0.000000000000000000, -0.000000000000000000 ) ) ;
#17161 = EDGE_CURVE ( 'NONE', #5638, #13804, #6291, .T. ) ;
#17162 = CARTESIAN_POINT ( 'NONE',  ( 4.999999999999999112, -32.11449294037157642, -54.20017844242546090 ) ) ;
#17163 = CARTESIAN_POINT ( 'NONE',  ( 10.00000000000000000, 6.681932690257323060, -25.38428207620315291 ) ) ;
#17164 = PRESENTATION_LAYER_ASSIGNMENT (  '', '', ( #14714 ) ) ;
#17165 = ADVANCED_FACE ( 'NONE', ( #11912 ), #10394, .T. ) ;
#17166 = VERTEX_POINT ( 'NONE', #4768 ) ;
#17167 = ORIENTED_EDGE ( 'NONE', *, *, #5419, .F. ) ;
#17168 = DIRECTION ( 'NONE',  ( 0.000000000000000000, -0.1564344650402170467, -0.9876883405951398798 ) ) ;
#17169 = DIRECTION ( 'NONE',  ( 2.220446049250313081E-16, -0.000000000000000000, -1.000000000000000000 ) ) ;
#17170 = EDGE_CURVE ( 'NONE', #7319, #202, #17723, .T. ) ;
#17171 = ORIENTED_EDGE ( 'NONE', *, *, #7145, .T. ) ;
#17172 = FILL_AREA_STYLE_COLOUR ( '', #882 ) ;
#17173 = CARTESIAN_POINT ( 'NONE',  ( 5.000000000000000000, -4.007856633822952652, -62.87238730325625369 ) ) ;
#17174 = CYLINDRICAL_SURFACE ( 'NONE', #17579, 2.649999999999999467 ) ;
#17175 = CARTESIAN_POINT ( 'NONE',  ( 2.500000000000000000, 2.357898499370432166, -2.385244779468109755E-15 ) ) ;
#17176 = CARTESIAN_POINT ( 'NONE',  ( -26.29305231718584324, -30.00000000000000000, 21.75302069950530637 ) ) ;
#17177 = VERTEX_POINT ( 'NONE', #13252 ) ;
#17178 = CARTESIAN_POINT ( 'NONE',  ( -117.1020693116508085, -30.00000000000000000, 17.04080595179778967 ) ) ;
#17179 = EDGE_LOOP ( 'NONE', ( #6069, #330, #6505, #631 ) ) ;
#17180 = ADVANCED_FACE ( 'NONE', ( #6008 ), #11830, .T. ) ;
#17181 = CARTESIAN_POINT ( 'NONE',  ( 5.000000000000000000, -57.83923611457302627, -24.97244012287564274 ) ) ;
#17182 = DIRECTION ( 'NONE',  ( -0.08031988216184954288, 0.000000000000000000, -0.9967691390334607604 ) ) ;
#17183 = VERTEX_POINT ( 'NONE', #10671 ) ;
#17184 = DIRECTION ( 'NONE',  ( 0.000000000000000000, 1.000000000000000000, 3.469446951950144779E-15 ) ) ;
#17185 = PRODUCT_CONTEXT ( 'NONE', #1708, 'mechanical' ) ;
#17186 = CARTESIAN_POINT ( 'NONE',  ( 0.000000000000000000, 50.71018745830443919, 24.33982105418919417 ) ) ;
#17187 = ORIENTED_EDGE ( 'NONE', *, *, #18177, .T. ) ;
#17188 =( REPRESENTATION_RELATIONSHIP ('NONE','NONE', #11014, #8256 ) REPRESENTATION_RELATIONSHIP_WITH_TRANSFORMATION ( #6115 )SHAPE_REPRESENTATION_RELATIONSHIP( ) );
#17189 = EDGE_CURVE ( 'NONE', #14080, #16577, #17639, .T. ) ;
#17190 = AXIS2_PLACEMENT_3D ( 'NONE', #13112, #14710, #5857 ) ;
#17191 = DIRECTION ( 'NONE',  ( 0.000000000000000000, 0.9876883405951382144, -0.1564344650402274828 ) ) ;
#17192 = DIRECTION ( 'NONE',  ( -0.000000000000000000, 1.000000000000000000, -0.000000000000000000 ) ) ;
#17193 = DIRECTION ( 'NONE',  ( -1.000000000000000000, -0.000000000000000000, -0.000000000000000000 ) ) ;
#17194 = CARTESIAN_POINT ( 'NONE',  ( 0.000000000000000000, -22.07705612348849655, 14.19907017806860949 ) ) ;
#17195 = FACE_OUTER_BOUND ( 'NONE', #6199, .T. ) ;
#17196 = EDGE_LOOP ( 'NONE', ( #8553, #2778, #9021, #2771 ) ) ;
#17197 = CARTESIAN_POINT ( 'NONE',  ( 10.00000000000000000, -12.18267823974732522, -25.42247726998028057 ) ) ;
#17198 = DIRECTION ( 'NONE',  ( -1.000000000000000000, 0.000000000000000000, -0.000000000000000000 ) ) ;
#17199 = DIRECTION ( 'NONE',  ( -1.000000000000000000, -0.000000000000000000, -0.000000000000000000 ) ) ;
#17200 = DIRECTION ( 'NONE',  ( -1.000000000000000000, -0.000000000000000000, -0.000000000000000000 ) ) ;
#17201 = ORIENTED_EDGE ( 'NONE', *, *, #9274, .T. ) ;
#17202 = ORIENTED_EDGE ( 'NONE', *, *, #2281, .T. ) ;
#17203 = AXIS2_PLACEMENT_3D ( 'NONE', #10602, #1842, #6218 ) ;
#17204 = CYLINDRICAL_SURFACE ( 'NONE', #14173, 2.649999999999999467 ) ;
#17205 = ORIENTED_EDGE ( 'NONE', *, *, #12608, .T. ) ;
#17206 = DIRECTION ( 'NONE',  ( -0.000000000000000000, 1.000000000000000000, -0.000000000000000000 ) ) ;
#17207 = EDGE_CURVE ( 'NONE', #4363, #17227, #3396, .T. ) ;
#17208 = VECTOR ( 'NONE', #5128, 1000.000000000000000 ) ;
#17209 = LINE ( 'NONE', #14627, #17210 ) ;
#17210 = VECTOR ( 'NONE', #17479, 1000.000000000000114 ) ;
#17212 = VECTOR ( 'NONE', #15250, 1000.000000000000114 ) ;
#17211 = DIRECTION ( 'NONE',  ( -1.000000000000000000, 0.000000000000000000, 0.000000000000000000 ) ) ;
#17213 = ORIENTED_EDGE ( 'NONE', *, *, #4303, .F. ) ;
#17214 = DIRECTION ( 'NONE',  ( -1.000000000000000000, 0.000000000000000000, 0.000000000000000000 ) ) ;
#17215 = ORIENTED_EDGE ( 'NONE', *, *, #16589, .F. ) ;
#17217 = CYLINDRICAL_SURFACE ( 'NONE', #7524, 2.649999999999992806 ) ;
#17216 = PRODUCT_DEFINITION_CONTEXT ( 'detailed design', #18627, 'design' ) ;
#17218 = FACE_BOUND ( 'NONE', #8355, .T. ) ;
#17219 = VERTEX_POINT ( 'NONE', #16207 ) ;
#17220 = CARTESIAN_POINT ( 'NONE',  ( 0.000000000000000000, -44.70888270294135936, -34.13306034420235591 ) ) ;
#17221 = ORIENTED_EDGE ( 'NONE', *, *, #18549, .F. ) ;
#17222 = ADVANCED_FACE ( 'NONE', ( #4585 ), #3444, .F. ) ;
#17223 = FACE_OUTER_BOUND ( 'NONE', #4040, .T. ) ;
#17224 = DIRECTION ( 'NONE',  ( 0.000000000000000000, 0.000000000000000000, 1.000000000000000000 ) ) ;
#17225 = AXIS2_PLACEMENT_3D ( 'NONE', #15215, #9773, #16919 ) ;
#17226 = VERTEX_POINT ( 'NONE', #7627 ) ;
#17227 = VERTEX_POINT ( 'NONE', #3354 ) ;
#17228 = AXIS2_PLACEMENT_3D ( 'NONE', #3281, #7737, #11759 ) ;
#17229 = CARTESIAN_POINT ( 'NONE',  ( 10.00000000000000000, 58.55669782892461228, 23.24033432160457835 ) ) ;
#17230 = EDGE_CURVE ( 'NONE', #10404, #9088, #2801, .T. ) ;
#17231 =( NAMED_UNIT ( * ) PLANE_ANGLE_UNIT ( ) SI_UNIT ( $, .RADIAN. ) );
#17232 = VERTEX_POINT ( 'NONE', #15981 ) ;
#17233 = CARTESIAN_POINT ( 'NONE',  ( 10.00000000000000000, 18.64666490672371424, 53.06836994729241042 ) ) ;
#17234 = DIRECTION ( 'NONE',  ( 1.000000000000000000, 0.000000000000000000, 0.000000000000000000 ) ) ;
#17235 = AXIS2_PLACEMENT_3D ( 'NONE', #15370, #8607, #17191 ) ;
#17236 = AXIS2_PLACEMENT_3D ( 'NONE', #9391, #15293, #2240 ) ;
#17237 = CIRCLE ( 'NONE', #14483, 5.000000000000004441 ) ;
#17238 = DIRECTION ( 'NONE',  ( -1.000000000000000000, -0.000000000000000000, -0.000000000000000000 ) ) ;
#17239 = AXIS2_PLACEMENT_3D ( 'NONE', #8330, #4137, #14125 ) ;
#17240 = COLOUR_RGB ( '',1.000000000000000000, 0.9490196078431372140, 0.9098039215686274384 ) ;
#17241 = EDGE_LOOP ( 'NONE', ( #18777, #948 ) ) ;
#17242 = VECTOR ( 'NONE', #304, 1000.000000000000000 ) ;
#17243 = VECTOR ( 'NONE', #6977, 1000.000000000000000 ) ;
#17244 = ORIENTED_EDGE ( 'NONE', *, *, #15524, .T. ) ;
#17245 = CARTESIAN_POINT ( 'NONE',  ( 13.90576474687299680, 10.00000000000000000, 42.79754323328179311 ) ) ;
#17246 = FACE_OUTER_BOUND ( 'NONE', #15525, .T. ) ;
#17247 = PLANE ( 'NONE',  #1741 ) ;
#17248 = FACE_BOUND ( 'NONE', #10107, .T. ) ;
#17249 = CARTESIAN_POINT ( 'NONE',  ( -90.00000000009001155, -34.99999999999999289, -1.301042606982605321E-15 ) ) ;
#17250 = DIRECTION ( 'NONE',  ( -1.000000000000000000, -0.000000000000000000, -0.000000000000000000 ) ) ;
#17251 = FACE_OUTER_BOUND ( 'NONE', #16767, .T. ) ;
#17252 = ORIENTED_EDGE ( 'NONE', *, *, #6549, .F. ) ;
#17253 = LINE ( 'NONE', #8574, #3961 ) ;
#17254 = SURFACE_STYLE_FILL_AREA ( #7418 ) ;
#17255 = LINE ( 'NONE', #17162, #18518 ) ;
#17256 = ORIENTED_EDGE ( 'NONE', *, *, #9100, .T. ) ;
#17257 = VECTOR ( 'NONE', #11240, 1000.000000000000000 ) ;
#17258 = AXIS2_PLACEMENT_3D ( 'NONE', #2554, #6838, #17140 ) ;
#17259 = CIRCLE ( 'NONE', #16025, 24.00000000002399858 ) ;
#17260 = ORIENTED_EDGE ( 'NONE', *, *, #12735, .T. ) ;
#17261 = AXIS2_PLACEMENT_3D ( 'NONE', #2350, #15308, #14158 ) ;
#17262 = CIRCLE ( 'NONE', #6588, 2.100000000000000089 ) ;
#17263 = EDGE_CURVE ( 'NONE', #9630, #6348, #5709, .T. ) ;
#17264 = ORIENTED_EDGE ( 'NONE', *, *, #15478, .F. ) ;
#17265 = DIRECTION ( 'NONE',  ( -1.000000000000000000, 0.000000000000000000, 0.000000000000000000 ) ) ;
#17266 = EDGE_CURVE ( 'NONE', #15951, #12029, #17506, .T. ) ;
#17267 = CYLINDRICAL_SURFACE ( 'NONE', #17365, 56.24900000005625600 ) ;
#17268 = CIRCLE ( 'NONE', #5996, 2.649999999999995914 ) ;
#17269 = ORIENTED_EDGE ( 'NONE', *, *, #14389, .F. ) ;
#17270 = CYLINDRICAL_SURFACE ( 'NONE', #16695, 4.250000000000000000 ) ;
#17271 = DIRECTION ( 'NONE',  ( 0.000000000000000000, 0.000000000000000000, 1.000000000000000000 ) ) ;
#17272 = VECTOR ( 'NONE', #9213, 1000.000000000000000 ) ;
#17273 = ADVANCED_FACE ( 'NONE', ( #4551 ), #15808, .F. ) ;
#17274 = CARTESIAN_POINT ( 'NONE',  ( -11.25000000000000533, 0.000000000000000000, 29.90000000000000213 ) ) ;
#17275 = CYLINDRICAL_SURFACE ( 'NONE', #1867, 2.649999999999992806 ) ;
#17276 = AXIS2_PLACEMENT_3D ( 'NONE', #1765, #1859, #3585 ) ;
#17277 = CARTESIAN_POINT ( 'NONE',  ( 2.000000000000000000, -6.429618962271402616, -1.000000000000000000 ) ) ;
#17278 = ORIENTED_EDGE ( 'NONE', *, *, #2891, .T. ) ;
#17279 = AXIS2_PLACEMENT_3D ( 'NONE', #3699, #9498, #849 ) ;
#17280 = CARTESIAN_POINT ( 'NONE',  ( 12.49999999999999289, 3.429011037612590065E-15, 28.00000000000001066 ) ) ;
#17281 = VERTEX_POINT ( 'NONE', #11415 ) ;
#17282 = EDGE_CURVE ( 'NONE', #9794, #3613, #8268, .T. ) ;
#17283 = CARTESIAN_POINT ( 'NONE',  ( 0.000000000000000000, -13.75000000000000533, 0.000000000000000000 ) ) ;
#17284 = DIRECTION ( 'NONE',  ( -1.000000000000000000, -0.000000000000000000, -0.000000000000000000 ) ) ;
#17285 = VERTEX_POINT ( 'NONE', #5609 ) ;
#17286 = APPLICATION_PROTOCOL_DEFINITION ( 'draft international standard', 'automotive_design', 1998, #16684 ) ;
#17287 = LINE ( 'NONE', #12604, #16648 ) ;
#17288 = ORIENTED_EDGE ( 'NONE', *, *, #16328, .T. ) ;
#17289 = EDGE_CURVE ( 'NONE', #11035, #16857, #8862, .T. ) ;
#17290 = VECTOR ( 'NONE', #15090, 1000.000000000000000 ) ;
#17291 = CIRCLE ( 'NONE', #16666, 33.00000000003299760 ) ;
#17292 = AXIS2_PLACEMENT_3D ( 'NONE', #16017, #7343, #8588 ) ;
#17293 = EDGE_CURVE ( 'NONE', #9928, #8389, #668, .T. ) ;
#17294 = CARTESIAN_POINT ( 'NONE',  ( 10.00000000000000000, 19.44239304137403579, -20.41355805489595454 ) ) ;
#17295 = ADVANCED_FACE ( 'NONE', ( #2761 ), #4192, .F. ) ;
#17296 = CARTESIAN_POINT ( 'NONE',  ( -90.00000000009001155, -88.00000000000000000, -27.50000000000000000 ) ) ;
#17297 = DIRECTION ( 'NONE',  ( 0.03086419753086420623, -0.9995235871707959241, 0.000000000000000000 ) ) ;
#17298 = DIRECTION ( 'NONE',  ( 0.000000000000000000, 0.000000000000000000, 1.000000000000000000 ) ) ;
#17299 = ADVANCED_FACE ( 'NONE', ( #16173 ), #3040, .T. ) ;
#17300 = DIRECTION ( 'NONE',  ( -1.000000000000000000, 0.000000000000000000, -0.000000000000000000 ) ) ;
#17301 = ORIENTED_EDGE ( 'NONE', *, *, #14797, .F. ) ;
#17302 = EDGE_CURVE ( 'NONE', #13804, #3659, #7970, .T. ) ;
#17303 = VECTOR ( 'NONE', #17352, 1000.000000000000000 ) ;
#17304 = CARTESIAN_POINT ( 'NONE',  ( 0.000000000000000000, 29.75305054077492173, -14.27431201565494767 ) ) ;
#17305 = LINE ( 'NONE', #4256, #15931 ) ;
#17306 = CARTESIAN_POINT ( 'NONE',  ( 0.000000000000000000, 16.60877409751197575, -20.32630374611166957 ) ) ;
#17307 = AXIS2_PLACEMENT_3D ( 'NONE', #5162, #8586, #9921 ) ;
#17308 = ORIENTED_EDGE ( 'NONE', *, *, #15622, .F. ) ;
#17309 = ORIENTED_EDGE ( 'NONE', *, *, #18415, .F. ) ;
#17310 = AXIS2_PLACEMENT_3D ( 'NONE', #8950, #17722, #16293 ) ;
#17311 = CARTESIAN_POINT ( 'NONE',  ( 0.000000000000000000, -32.46095361140696411, 5.940243314904091854 ) ) ;
#17312 = SURFACE_SIDE_STYLE ('',( #10239 ) ) ;
#17313 = ORIENTED_EDGE ( 'NONE', *, *, #14704, .T. ) ;
#17314 = AXIS2_PLACEMENT_3D ( 'NONE', #11286, #8435, #18619 ) ;
#17315 = AXIS2_PLACEMENT_3D ( 'NONE', #12086, #1530, #4854 ) ;
#17316 = CARTESIAN_POINT ( 'NONE',  ( 10.04305231718605285, -26.50000000000000000, -33.55933677959240669 ) ) ;
#17317 = CIRCLE ( 'NONE', #4825, 26.24900000002625333 ) ;
#17318 = CYLINDRICAL_SURFACE ( 'NONE', #10258, 27.29487558977753991 ) ;
#17319 = ORIENTED_EDGE ( 'NONE', *, *, #11917, .T. ) ;
#17320 = DIRECTION ( 'NONE',  ( -1.000000000000000000, 0.000000000000000000, -0.000000000000000000 ) ) ;
#17321 = ORIENTED_EDGE ( 'NONE', *, *, #18748, .F. ) ;
#17322 = DIRECTION ( 'NONE',  ( 0.000000000000000000, 0.000000000000000000, -1.000000000000000000 ) ) ;
#17323 = ORIENTED_EDGE ( 'NONE', *, *, #17120, .T. ) ;
#17324 = DIRECTION ( 'NONE',  ( -1.000000000000000000, 0.000000000000000000, 0.000000000000000000 ) ) ;
#17325 = ADVANCED_FACE ( 'NONE', ( #7221 ), #13756, .F. ) ;
#17326 = ORIENTED_EDGE ( 'NONE', *, *, #7697, .F. ) ;
#17327 = CARTESIAN_POINT ( 'NONE',  ( 10.00000000000000000, -32.70783759231083110, -4.381479206523328784 ) ) ;
#17328 = CARTESIAN_POINT ( 'NONE',  ( -27.29487558977753991, 1.305124410222464393, 0.000000000000000000 ) ) ;
#17329 = CIRCLE ( 'NONE', #12158, 26.24900000002625333 ) ;
#17330 = VERTEX_POINT ( 'NONE', #10363 ) ;
#17331 = VERTEX_POINT ( 'NONE', #15895 ) ;
#17332 = FACE_OUTER_BOUND ( 'NONE', #6615, .T. ) ;
#17333 = CIRCLE ( 'NONE', #10319, 25.10000000000000142 ) ;
#17334 = ORIENTED_EDGE ( 'NONE', *, *, #10525, .F. ) ;
#17335 = CYLINDRICAL_SURFACE ( 'NONE', #2718, 12.00000000001200462 ) ;
#17336 = DIRECTION ( 'NONE',  ( -0.000000000000000000, 1.000000000000000000, -0.000000000000000000 ) ) ;
#17337 = CIRCLE ( 'NONE', #9109, 2.500000000000000444 ) ;
#17338 = ORIENTED_EDGE ( 'NONE', *, *, #8664, .T. ) ;
#17339=STYLED_ITEM('',(#18876),#9242);
#17340 = ORIENTED_EDGE ( 'NONE', *, *, #11844, .F. ) ;
#17341 = DIRECTION ( 'NONE',  ( 0.000000000000000000, 0.000000000000000000, 1.000000000000000000 ) ) ;
#17342 = DIRECTION ( 'NONE',  ( -1.000000000000000000, 0.000000000000000000, 0.000000000000000000 ) ) ;
#17343 = DIRECTION ( 'NONE',  ( 1.000000000000000000, 0.000000000000000000, 0.000000000000000000 ) ) ;
#17344 = CARTESIAN_POINT ( 'NONE',  ( 0.000000000000000000, 7.813799127874054840, -55.83748330407399152 ) ) ;
#17345 = ADVANCED_FACE ( 'NONE', ( #7404 ), #14649, .F. ) ;
#17346 = FACE_OUTER_BOUND ( 'NONE', #13478, .T. ) ;
#17347 = DIRECTION ( 'NONE',  ( 0.000000000000000000, 0.000000000000000000, 1.000000000000000000 ) ) ;
#17348 = FACE_BOUND ( 'NONE', #5259, .T. ) ;
#17349 = ORIENTED_EDGE ( 'NONE', *, *, #16616, .T. ) ;
#17350 = CARTESIAN_POINT ( 'NONE',  ( -1.287237434361707233, -3.875615274277397937, -3.430618716626816500 ) ) ;
#17351 = EDGE_LOOP ( 'NONE', ( #15048, #11365, #13473, #18154 ) ) ;
#17352 = DIRECTION ( 'NONE',  ( 0.000000000000000000, -1.000000000000000000, 1.287488025362403787E-15 ) ) ;
#17353 = VECTOR ( 'NONE', #4063, 1000.000000000000000 ) ;
#17354 = LINE ( 'NONE', #2868, #386 ) ;
#17355 = AXIS2_PLACEMENT_3D ( 'NONE', #4054, #9853, #15663 ) ;
#17356 = VERTEX_POINT ( 'NONE', #5973 ) ;
#17357 = ADVANCED_FACE ( 'NONE', ( #8739 ), #2847, .T. ) ;
#17358 = VERTEX_POINT ( 'NONE', #178 ) ;
#17359 = EDGE_CURVE ( 'NONE', #16921, #13860, #1892, .T. ) ;
#17360 = FACE_OUTER_BOUND ( 'NONE', #1578, .T. ) ;
#17361 = CARTESIAN_POINT ( 'NONE',  ( 10.00000000000000178, 0.000000000000000000, 30.00000000000000000 ) ) ;
#17362 = VERTEX_POINT ( 'NONE', #5800 ) ;
#17363 =( NAMED_UNIT ( * ) PLANE_ANGLE_UNIT ( ) SI_UNIT ( $, .RADIAN. ) );
#17364 = CARTESIAN_POINT ( 'NONE',  ( 10.00000000000000000, 7.478235706489787304, -55.74967257055874370 ) ) ;
#17365 = AXIS2_PLACEMENT_3D ( 'NONE', #983, #18303, #4116 ) ;
#17366 = CARTESIAN_POINT ( 'NONE',  ( 10.00000000000000000, 26.20671763660628528, 1.489278925039608570 ) ) ;
#17367 = CARTESIAN_POINT ( 'NONE',  ( 10.00000000000000000, 56.23315539212690339, 1.335003989221828835 ) ) ;
#17368 = DIRECTION ( 'NONE',  ( 0.000000000000000000, 0.000000000000000000, 1.000000000000000000 ) ) ;
#17369 = VERTEX_POINT ( 'NONE', #7122 ) ;
#17370 = CARTESIAN_POINT ( 'NONE',  ( -0.5000000000000000000, -30.39588787977742257, -2.000000000000000000 ) ) ;
#17371 = ORIENTED_EDGE ( 'NONE', *, *, #14953, .F. ) ;
#17372 = CYLINDRICAL_SURFACE ( 'NONE', #9540, 56.24900000005625600 ) ;
#17373 = CARTESIAN_POINT ( 'NONE',  ( 10.00000000000000000, -24.97244012287460535, -57.83923611457345970 ) ) ;
#17374 = ORIENTED_EDGE ( 'NONE', *, *, #1783, .F. ) ;
#17375 = EDGE_CURVE ( 'NONE', #8784, #10053, #13135, .T. ) ;
#17376 = VERTEX_POINT ( 'NONE', #11702 ) ;
#17377 = AXIS2_PLACEMENT_3D ( 'NONE', #13071, #11904, #26 ) ;
#17378 = DIRECTION ( 'NONE',  ( 0.000000000000000000, 1.000000000000000000, 0.000000000000000000 ) ) ;
#17379 = CARTESIAN_POINT ( 'NONE',  ( 2.500000000000000000, 2.357898499370431722, -2.818925648462311528E-15 ) ) ;
#17380 = LINE ( 'NONE', #12906, #17883 ) ;
#17381 = DIRECTION ( 'NONE',  ( 0.000000000000000000, 0.000000000000000000, 1.000000000000000000 ) ) ;
#17382 = DIRECTION ( 'NONE',  ( 0.000000000000000000, -0.5877852522924623679, -0.8090169943749552228 ) ) ;
#17383 = ORIENTED_EDGE ( 'NONE', *, *, #12963, .T. ) ;
#17384 = AXIS2_PLACEMENT_3D ( 'NONE', #3024, #10347, #10249 ) ;
#17385 = CARTESIAN_POINT ( 'NONE',  ( -117.1020693116506379, -34.99999999999999289, -19.69080595179801207 ) ) ;
#17386 = CARTESIAN_POINT ( 'NONE',  ( 10.00000000000000000, -27.72801475327278453, 6.913036516934497833 ) ) ;
#17387 = DIRECTION ( 'NONE',  ( 0.000000000000000000, 0.000000000000000000, 1.000000000000000000 ) ) ;
#17388 = ORIENTED_EDGE ( 'NONE', *, *, #9228, .F. ) ;
#17389 = ORIENTED_EDGE ( 'NONE', *, *, #4086, .T. ) ;
#17390 = EDGE_CURVE ( 'NONE', #16165, #16942, #18581, .T. ) ;
#17391 = ADVANCED_FACE ( 'NONE', ( #2388 ), #7049, .F. ) ;
#17392 = CARTESIAN_POINT ( 'NONE',  ( -90.00000000009001155, -13.00000000000001776, -1.691355389077386325E-15 ) ) ;
#17393 =( NAMED_UNIT ( * ) SI_UNIT ( $, .STERADIAN. ) SOLID_ANGLE_UNIT ( ) );
#17394 = AXIS2_PLACEMENT_3D ( 'NONE', #4315, #18690, #5829 ) ;
#17395 = EDGE_CURVE ( 'NONE', #484, #10707, #13461, .T. ) ;
#17396 = EDGE_LOOP ( 'NONE', ( #7251, #17672, #12647, #17326 ) ) ;
#17397 = EDGE_CURVE ( 'NONE', #7573, #7040, #5235, .T. ) ;
#17398 = EDGE_CURVE ( 'NONE', #657, #1081, #15437, .T. ) ;
#17399 = CARTESIAN_POINT ( 'NONE',  ( 10.00000000000000000, 0.000000000000000000, 0.000000000000000000 ) ) ;
#17400 = CIRCLE ( 'NONE', #3406, 56.24900000005625600 ) ;
#17401 = CARTESIAN_POINT ( 'NONE',  ( 5.000000000000000000, 40.19788616105680035, -48.50907078259338334 ) ) ;
#17402 = ORIENTED_EDGE ( 'NONE', *, *, #7041, .F. ) ;
#17403 = EDGE_CURVE ( 'NONE', #17733, #2703, #11926, .T. ) ;
#17404 = ORIENTED_EDGE ( 'NONE', *, *, #6778, .T. ) ;
#17405 = CARTESIAN_POINT ( 'NONE',  ( 10.00000000000000000, -18.38754094778203552, -53.29895248911694239 ) ) ;
#17406 = ORIENTED_EDGE ( 'NONE', *, *, #13257, .T. ) ;
#17407 = EDGE_LOOP ( 'NONE', ( #3737, #5700 ) ) ;
#17408 = DIRECTION ( 'NONE',  ( 0.000000000000000000, 0.000000000000000000, 1.000000000000000000 ) ) ;
#17409 = DIRECTION ( 'NONE',  ( -0.000000000000000000, 1.000000000000000000, -0.000000000000000000 ) ) ;
#17410 = VERTEX_POINT ( 'NONE', #5444 ) ;
#17411 = ORIENTED_EDGE ( 'NONE', *, *, #1792, .F. ) ;
#17412 = ADVANCED_BREP_SHAPE_REPRESENTATION ( '', ( #3693, #8017 ), #6229 ) ;
#17413 = EDGE_CURVE ( 'NONE', #5270, #2059, #8571, .T. ) ;
#17414 = DIRECTION ( 'NONE',  ( 0.000000000000000000, 0.3090169943749481174, -0.9510565162951533091 ) ) ;
#17415 = ORIENTED_EDGE ( 'NONE', *, *, #717, .T. ) ;
#17416 = DIRECTION ( 'NONE',  ( -1.000000000000000000, 0.000000000000000000, 0.000000000000000000 ) ) ;
#17417 = CIRCLE ( 'NONE', #381, 12.00000000001200462 ) ;
#17418 = EDGE_CURVE ( 'NONE', #9007, #3135, #2478, .T. ) ;
#17419 = DIRECTION ( 'NONE',  ( 0.9995004958639132076, 0.000000000000000000, 0.03160314490350067673 ) ) ;
#17420 = ORIENTED_EDGE ( 'NONE', *, *, #5272, .T. ) ;
#17421 = PRODUCT_DEFINITION_SHAPE ( 'NONE', 'NONE',  #18821 ) ;
#17422 = ORIENTED_EDGE ( 'NONE', *, *, #10084, .T. ) ;
#17423 = CARTESIAN_POINT ( 'NONE',  ( 0.000000000000000000, 0.000000000000000000, 0.000000000000000000 ) ) ;
#17424 = DIRECTION ( 'NONE',  ( 0.000000000000000000, 1.000000000000000000, 0.000000000000000000 ) ) ;
#17425 = CARTESIAN_POINT ( 'NONE',  ( 10.00000000000000000, 0.000000000000000000, 0.000000000000000000 ) ) ;
#17426 = DIRECTION ( 'NONE',  ( 1.000000000000000000, 0.000000000000000000, 0.000000000000000000 ) ) ;
#17427 = CARTESIAN_POINT ( 'NONE',  ( -4.000000000000000000, 1.677772373332757194, -3.535253723897187506 ) ) ;
#17428 = LINE ( 'NONE', #4379, #8190 ) ;
#17430 = VECTOR ( 'NONE', #9357, 1000.000000000000000 ) ;
#17429 = DIRECTION ( 'NONE',  ( 0.000000000000000000, -0.4539904997395542430, 0.8910065241883641241 ) ) ;
#17431 = DIRECTION ( 'NONE',  ( 0.000000000000000000, 0.000000000000000000, -1.000000000000000000 ) ) ;
#17432 = VERTEX_POINT ( 'NONE', #17071 ) ;
#17433 = CLOSED_SHELL ( 'NONE', ( #17742, #13198, #6402, #4875, #8291, #18471, #15073, #17942, #14713, #9918, #2030, #7782, #5298, #4343, #12258, #2851, #5621, #13199, #17826, #7594, #6620, #6506 ) ) ;
#17434 = CARTESIAN_POINT ( 'NONE',  ( 0.000000000000000000, -25.38428207620327370, 6.681932690256871865 ) ) ;
#17435 = CARTESIAN_POINT ( 'NONE',  ( 0.000000000000000000, 0.000000000000000000, 0.000000000000000000 ) ) ;
#17436 = ORIENTED_EDGE ( 'NONE', *, *, #10063, .T. ) ;
#17437 = DIRECTION ( 'NONE',  ( -1.000000000000000000, -0.000000000000000000, 0.000000000000000000 ) ) ;
#17438 = DIRECTION ( 'NONE',  ( 0.000000000000000000, 0.000000000000000000, -1.000000000000000000 ) ) ;
#17439 = ADVANCED_FACE ( 'NONE', ( #14382 ), #1254, .T. ) ;
#17440 = VECTOR ( 'NONE', #18428, 1000.000000000000000 ) ;
#17441 = CIRCLE ( 'NONE', #11037, 0.1000000000000028644 ) ;
#17442 = ORIENTED_EDGE ( 'NONE', *, *, #18560, .T. ) ;
#17443 = LINE ( 'NONE', #4391, #13276 ) ;
#17444 = CARTESIAN_POINT ( 'NONE',  ( 10.00000000000000000, 39.14194549634364506, 40.58063702438359144 ) ) ;
#17445 = ORIENTED_EDGE ( 'NONE', *, *, #8982, .T. ) ;
#17446 = FACE_OUTER_BOUND ( 'NONE', #9871, .T. ) ;
#17447 = CARTESIAN_POINT ( 'NONE',  ( 0.000000000000000000, -18.38754094778203552, -53.29895248911694239 ) ) ;
#17448 = DIRECTION ( 'NONE',  ( 0.000000000000000000, 0.000000000000000000, 1.000000000000000000 ) ) ;
#17449 = CARTESIAN_POINT ( 'NONE',  ( 0.000000000000000000, 10.00000000000000000, 0.000000000000000000 ) ) ;
#17450 = CARTESIAN_POINT ( 'NONE',  ( 0.000000000000000000, -13.75000000000000355, 0.000000000000000000 ) ) ;
#17451 = ORIENTED_EDGE ( 'NONE', *, *, #16059, .F. ) ;
#17452 = DIRECTION ( 'NONE',  ( -1.000000000000000000, 0.000000000000000000, 0.000000000000000000 ) ) ;
#17453 = VERTEX_POINT ( 'NONE', #18377 ) ;
#17454 = EDGE_CURVE ( 'NONE', #5476, #7932, #4325, .T. ) ;
#17455 = VECTOR ( 'NONE', #11667, 1000.000000000000000 ) ;
#17456 = FACE_BOUND ( 'NONE', #10365, .T. ) ;
#17457 = CARTESIAN_POINT ( 'NONE',  ( 4.999999999999997335, 5.204748896376250699E-16, -4.250000000000000000 ) ) ;
#17458 = ORIENTED_EDGE ( 'NONE', *, *, #10174, .F. ) ;
#17459 = APPLICATION_PROTOCOL_DEFINITION ( 'draft international standard', 'automotive_design', 1998, #14726 ) ;
#17460 = ADVANCED_FACE ( 'NONE', ( #14007 ), #11139, .T. ) ;
#17461 = ORIENTED_EDGE ( 'NONE', *, *, #5520, .F. ) ;
#17462 = AXIS2_PLACEMENT_3D ( 'NONE', #10976, #15358, #2313 ) ;
#17463 = LINE ( 'NONE', #5569, #13568 ) ;
#17464 = CARTESIAN_POINT ( 'NONE',  ( 10.00000000000000000, -50.71018745830461683, 24.33982105418882469 ) ) ;
#17465 = DIRECTION ( 'NONE',  ( 0.000000000000000000, 0.7071067811865440200, 0.7071067811865511255 ) ) ;
#17466 = FACE_OUTER_BOUND ( 'NONE', #16412, .T. ) ;
#17467 = FACE_OUTER_BOUND ( 'NONE', #1633, .T. ) ;
#17468 = CARTESIAN_POINT ( 'NONE',  ( 10.00000000000000000, 0.000000000000000000, 0.000000000000000000 ) ) ;
#17469 = VERTEX_POINT ( 'NONE', #9812 ) ;
#17470 = CARTESIAN_POINT ( 'NONE',  ( 10.00000000000000000, -32.70783759231088794, 4.381479206522872261 ) ) ;
#17471 = CARTESIAN_POINT ( 'NONE',  ( -90.00000000009003998, 1.000000000000018208, -5.746271514173173500E-15 ) ) ;
#17472 = CYLINDRICAL_SURFACE ( 'NONE', #12473, 27.50000000000000000 ) ;
#17473 = ORIENTED_EDGE ( 'NONE', *, *, #14448, .T. ) ;
#17474 = ORIENTED_EDGE ( 'NONE', *, *, #16358, .F. ) ;
#17475 = DIRECTION ( 'NONE',  ( -0.000000000000000000, 1.000000000000000000, -0.000000000000000000 ) ) ;
#17476 = CARTESIAN_POINT ( 'NONE',  ( 0.000000000000000000, 0.000000000000000000, 0.000000000000000000 ) ) ;
#17477 = ORIENTED_EDGE ( 'NONE', *, *, #12203, .F. ) ;
#17478 = AXIS2_PLACEMENT_3D ( 'NONE', #2258, #17981, #7976 ) ;
#17479 = DIRECTION ( 'NONE',  ( 0.1305261922200516844, 0.9914448613738103822, -0.000000000000000000 ) ) ;
#17480 = LINE ( 'NONE', #5947, #9273 ) ;
#17481 = CARTESIAN_POINT ( 'NONE',  ( -36.40576474687247099, 0.000000000000000000, 26.45033635316149301 ) ) ;
#17482 = ORIENTED_EDGE ( 'NONE', *, *, #11695, .T. ) ;
#17483 = EDGE_CURVE ( 'NONE', #10049, #13701, #15577, .T. ) ;
#17484 = CARTESIAN_POINT ( 'NONE',  ( 10.00000000000000000, 27.72801475327282361, -5.086963483077305170 ) ) ;
#17485 = AXIS2_PLACEMENT_3D ( 'NONE', #8238, #10981, #15565 ) ;
#17486 = EDGE_CURVE ( 'NONE', #14829, #14393, #7061, .T. ) ;
#17487 = VECTOR ( 'NONE', #8815, 1000.000000000000114 ) ;
#17488 = VERTEX_POINT ( 'NONE', #968 ) ;
#17489 = CARTESIAN_POINT ( 'NONE',  ( -1.250000000000000000, -6.429618962271402616, 0.000000000000000000 ) ) ;
#17490 = VECTOR ( 'NONE', #4695, 1000.000000000000000 ) ;
#17491 = ORIENTED_EDGE ( 'NONE', *, *, #15065, .T. ) ;
#17492 = ORIENTED_EDGE ( 'NONE', *, *, #4286, .F. ) ;
#17493 = EDGE_CURVE ( 'NONE', #6780, #3169, #17708, .T. ) ;
#17494 = DIRECTION ( 'NONE',  ( 2.031314180040284764E-16, 1.000000000000000000, 1.301042606982601377E-16 ) ) ;
#17495 = CARTESIAN_POINT ( 'NONE',  ( 4.211140560182196957, -2.431303136016555122, -3.745885042887436622 ) ) ;
#17496 = ORIENTED_EDGE ( 'NONE', *, *, #15230, .F. ) ;
#17497 = EDGE_LOOP ( 'NONE', ( #1834, #10923, #14575, #17135 ) ) ;
#17498 = FACE_OUTER_BOUND ( 'NONE', #8402, .T. ) ;
#17499 = EDGE_CURVE ( 'NONE', #4272, #684, #18481, .T. ) ;
#17500 = ORIENTED_EDGE ( 'NONE', *, *, #18405, .T. ) ;
#17501 = CARTESIAN_POINT ( 'NONE',  ( 0.000000000000000000, 5.876895005582427167, 62.72529079327809853 ) ) ;
#17502 = AXIS2_PLACEMENT_3D ( 'NONE', #6892, #12805, #16803 ) ;
#17503 = EDGE_CURVE ( 'NONE', #15464, #13103, #7355, .T. ) ;
#17504 = CIRCLE ( 'NONE', #3527, 12.00000000001200107 ) ;
#17505 = AXIS2_PLACEMENT_3D ( 'NONE', #4080, #4606, #10499 ) ;
#17506 = LINE ( 'NONE', #11524, #11909 ) ;
#17507 = ORIENTED_EDGE ( 'NONE', *, *, #16547, .F. ) ;
#17508 = EDGE_CURVE ( 'NONE', #2818, #1905, #5537, .T. ) ;
#17509 = EDGE_CURVE ( 'NONE', #17641, #17469, #10701, .T. ) ;
#17510 = AXIS2_PLACEMENT_3D ( 'NONE', #1116, #13971, #8348 ) ;
#17511 = ORIENTED_EDGE ( 'NONE', *, *, #4957, .T. ) ;
#17512 = DIRECTION ( 'NONE',  ( 1.000000000000000000, 0.000000000000000000, 0.000000000000000000 ) ) ;
#17513 = CARTESIAN_POINT ( 'NONE',  ( 10.00000000000000000, -9.823366686501049827, 55.51919907100648999 ) ) ;
#17514 = CARTESIAN_POINT ( 'NONE',  ( 10.00000000000000000, -25.38428207620327370, 6.681932690256871865 ) ) ;
#17515 = VERTEX_POINT ( 'NONE', #18763 ) ;
#17516 = DIRECTION ( 'NONE',  ( 0.000000000000000000, -0.8910065241883722287, 0.4539904997395383668 ) ) ;
#17517 = CARTESIAN_POINT ( 'NONE',  ( 10.00000000000000000, 0.000000000000000000, 0.000000000000000000 ) ) ;
#17518 = DIRECTION ( 'NONE',  ( 0.000000000000000000, 0.000000000000000000, -1.000000000000000000 ) ) ;
#17519 = CIRCLE ( 'NONE', #190, 26.24900000002624978 ) ;
#17520 = CARTESIAN_POINT ( 'NONE',  ( 0.000000000000000000, 10.00000000000000000, -150.0000000000000284 ) ) ;
#17521 = ORIENTED_EDGE ( 'NONE', *, *, #9059, .T. ) ;
#17522 = CARTESIAN_POINT ( 'NONE',  ( 10.00000000000000000, 9.823366686500662581, 55.51919907100656104 ) ) ;
#17523 = AXIS2_PLACEMENT_3D ( 'NONE', #10672, #6678, #5146 ) ;
#17524 = ADVANCED_FACE ( 'NONE', ( #10097 ), #13231, .T. ) ;
#17525 = FILL_AREA_STYLE_COLOUR ( '', #17240 ) ;
#17526 = ORIENTED_EDGE ( 'NONE', *, *, #10964, .T. ) ;
#17527 = CARTESIAN_POINT ( 'NONE',  ( 10.04305231718605285, -26.50000000000000000, -28.25933677959240953 ) ) ;
#17528 = DIRECTION ( 'NONE',  ( -1.000000000000000000, 0.000000000000000000, -0.000000000000000000 ) ) ;
#17529 = ITEM_DEFINED_TRANSFORMATION ( 'NONE', 'NONE', #11412,  #8017 ) ;
#17530 = VECTOR ( 'NONE', #2045, 1000.000000000000000 ) ;
#17531 = CIRCLE ( 'NONE', #5053, 0.7499999999999997780 ) ;
#17532 = AXIS2_PLACEMENT_3D ( 'NONE', #8251, #15489, #2334 ) ;
#17533 = ORIENTED_EDGE ( 'NONE', *, *, #4266, .T. ) ;
#17534 = CARTESIAN_POINT ( 'NONE',  ( -90.00000000009001155, -88.00000000000000000, 27.50000000000000000 ) ) ;
#17535 = CARTESIAN_POINT ( 'NONE',  ( 10.00000000000000000, -25.38428207620317778, -6.681932690257235130 ) ) ;
#17536 = ORIENTED_EDGE ( 'NONE', *, *, #5572, .T. ) ;
#17537 = CARTESIAN_POINT ( 'NONE',  ( 0.000000000000000000, -40.70683587897985234, 38.81885513159974010 ) ) ;
#17538 =( REPRESENTATION_RELATIONSHIP ('NONE','NONE', #11014, #16765 ) REPRESENTATION_RELATIONSHIP_WITH_TRANSFORMATION ( #14976 )SHAPE_REPRESENTATION_RELATIONSHIP( ) );
#17539 = CARTESIAN_POINT ( 'NONE',  ( 0.000000000000000000, 16.10733642026482570, 53.89344778774818678 ) ) ;
#17540 = DIRECTION ( 'NONE',  ( -1.000000000000000000, 0.000000000000000000, 0.000000000000000000 ) ) ;
#17541 = LINE ( 'NONE', #13078, #13134 ) ;
#17542 = VECTOR ( 'NONE', #7505, 1000.000000000000000 ) ;
#17543 = CARTESIAN_POINT ( 'NONE',  ( 10.00000000000000000, 3.730438010304726770, -27.94286728106388296 ) ) ;
#17544 = ORIENTED_EDGE ( 'NONE', *, *, #18358, .F. ) ;
#17545 = CARTESIAN_POINT ( 'NONE',  ( 0.000000000000000000, 0.5192545390863916310, -1.000000000000000000 ) ) ;
#17546 = ORIENTED_EDGE ( 'NONE', *, *, #4591, .F. ) ;
#17547 = EDGE_CURVE ( 'NONE', #8173, #16278, #12954, .T. ) ;
#17548 = AXIS2_PLACEMENT_3D ( 'NONE', #12772, #1252, #6852 ) ;
#17549 = PLANE ( 'NONE',  #15772 ) ;
#17550 = EDGE_LOOP ( 'NONE', ( #11624, #14422, #13157, #3845 ) ) ;
#17551 = AXIS2_PLACEMENT_3D ( 'NONE', #203, #14761, #16643 ) ;
#17552 = VECTOR ( 'NONE', #16673, 1000.000000000000000 ) ;
#17553 = APPLICATION_PROTOCOL_DEFINITION ( 'draft international standard', 'automotive_design', 1998, #9758 ) ;
#17554 = ORIENTED_EDGE ( 'NONE', *, *, #14651, .T. ) ;
#17555 = VECTOR ( 'NONE', #3045, 1000.000000000000000 ) ;
#17556 = CIRCLE ( 'NONE', #12998, 24.00000000002399148 ) ;
#17557 = EDGE_CURVE ( 'NONE', #12292, #6749, #9801, .T. ) ;
#17558 = CYLINDRICAL_SURFACE ( 'NONE', #7788, 5.000000000000004441 ) ;
#17559 = DIRECTION ( 'NONE',  ( 0.1305261922200524616, 0.9914448613738103822, -0.000000000000000000 ) ) ;
#17560 = CIRCLE ( 'NONE', #11494, 24.00000000002399858 ) ;
#17561 = AXIS2_PLACEMENT_3D ( 'NONE', #11110, #2454, #12547 ) ;
#17562 = LINE ( 'NONE', #4328, #2682 ) ;
#17563 = DIRECTION ( 'NONE',  ( -0.000000000000000000, 1.000000000000000000, -0.000000000000000000 ) ) ;
#17564 = EDGE_CURVE ( 'NONE', #17376, #17771, #11006, .T. ) ;
#17565 = CARTESIAN_POINT ( 'NONE',  ( 10.00000000000000000, 0.000000000000000000, 0.000000000000000000 ) ) ;
#17566 = CARTESIAN_POINT ( 'NONE',  ( -10.00000000000000000, 0.000000000000000000, 0.000000000000000000 ) ) ;
#17567 = DIRECTION ( 'NONE',  ( 0.000000000000000000, 0.000000000000000000, 1.000000000000000000 ) ) ;
#17568 = EDGE_LOOP ( 'NONE', ( #8593, #12986, #17762, #15374 ) ) ;
#17569 = CARTESIAN_POINT ( 'NONE',  ( 10.00000000000000000, 27.72801475327274900, 5.086963483077687975 ) ) ;
#17570 = DIRECTION ( 'NONE',  ( -1.000000000000000000, 0.000000000000000000, 0.000000000000000000 ) ) ;
#17571 = DIRECTION ( 'NONE',  ( -1.000000000000000000, 0.000000000000000000, 0.000000000000000000 ) ) ;
#17572 = ORIENTED_EDGE ( 'NONE', *, *, #7563, .T. ) ;
#17573 = ORIENTED_EDGE ( 'NONE', *, *, #7511, .T. ) ;
#17574 = DIRECTION ( 'NONE',  ( 0.000000000000000000, -0.8910065241883626808, -0.4539904997395571296 ) ) ;
#17575 = VECTOR ( 'NONE', #18229, 1000.000000000000000 ) ;
#17576 = CARTESIAN_POINT ( 'NONE',  ( 3.309651814758564736, -5.455921364805393026, -1.000000000000000000 ) ) ;
#17577 = ORIENTED_EDGE ( 'NONE', *, *, #17963, .F. ) ;
#17578 = AXIS2_PLACEMENT_3D ( 'NONE', #7360, #12812, #18706 ) ;
#17579 = AXIS2_PLACEMENT_3D ( 'NONE', #5555, #2501, #11058 ) ;
#17580 = ADVANCED_FACE ( 'NONE', ( #189 ), #5988, .T. ) ;
#17581 = CARTESIAN_POINT ( 'NONE',  ( 5.000000000000000000, -23.88582760061497368, 22.76987570971518338 ) ) ;
#17582 = DIRECTION ( 'NONE',  ( -1.000000000000000000, -0.000000000000000000, -0.000000000000000000 ) ) ;
#17583 = DIRECTION ( 'NONE',  ( 0.000000000000000000, 0.000000000000000000, 1.000000000000000000 ) ) ;
#17584 = VERTEX_POINT ( 'NONE', #285 ) ;
#17585 = CARTESIAN_POINT ( 'NONE',  ( 10.00000000000000000, 53.22058882792196499, 33.71303790549294632 ) ) ;
#17586 = CIRCLE ( 'NONE', #9372, 4.799999999999999822 ) ;
#17587 = PRESENTATION_LAYER_ASSIGNMENT (  '', '', ( #10302 ) ) ;
#17588 = VERTEX_POINT ( 'NONE', #9031 ) ;
#17589 = DIRECTION ( 'NONE',  ( -1.000000000000000000, 0.000000000000000000, -0.000000000000000000 ) ) ;
#17590 = VERTEX_POINT ( 'NONE', #10372 ) ;
#17591 = VERTEX_POINT ( 'NONE', #3051 ) ;
#17592 = CARTESIAN_POINT ( 'NONE',  ( 5.000000000000000000, -53.22058882792172341, -33.71303790549333712 ) ) ;
#17593 = CARTESIAN_POINT ( 'NONE',  ( 4.888507282057958925, -29.45674523562211888, -2.000000000000000000 ) ) ;
#17594 = ORIENTED_EDGE ( 'NONE', *, *, #9778, .F. ) ;
#17595 = ORIENTED_EDGE ( 'NONE', *, *, #1120, .F. ) ;
#17596 = DIRECTION ( 'NONE',  ( 0.000000000000000000, 0.000000000000000000, 1.000000000000000000 ) ) ;
#17597 = VERTEX_POINT ( 'NONE', #6085 ) ;
#17598 = DIRECTION ( 'NONE',  ( -1.000000000000000000, -0.000000000000000000, -0.000000000000000000 ) ) ;
#17599 = EDGE_CURVE ( 'NONE', #16028, #10905, #11627, .T. ) ;
#17600 = AXIS2_PLACEMENT_3D ( 'NONE', #15424, #12471, #11027 ) ;
#17601 = EDGE_CURVE ( 'NONE', #3677, #11456, #1524, .T. ) ;
#17602 = AXIS2_PLACEMENT_3D ( 'NONE', #3809, #18191, #16569 ) ;
#17603 = AXIS2_PLACEMENT_3D ( 'NONE', #16552, #3509, #3230 ) ;
#17604 = DIRECTION ( 'NONE',  ( 1.000000000000000000, 0.000000000000000000, 0.000000000000000000 ) ) ;
#17605 = ORIENTED_EDGE ( 'NONE', *, *, #2482, .F. ) ;
#17606 = AXIS2_PLACEMENT_3D ( 'NONE', #3357, #9151, #4588 ) ;
#17607 = VERTEX_POINT ( 'NONE', #11807 ) ;
#17608 = DIRECTION ( 'NONE',  ( -1.000000000000000000, -0.000000000000000000, -0.000000000000000000 ) ) ;
#17609 = CARTESIAN_POINT ( 'NONE',  ( 10.00000000000000000, -26.45033635316118747, 36.40576474687271258 ) ) ;
#17610 = CARTESIAN_POINT ( 'NONE',  ( 10.00000000000000000, 53.89344778774834310, -16.10733642026427148 ) ) ;
#17611 = ORIENTED_EDGE ( 'NONE', *, *, #17302, .T. ) ;
#17612 = CARTESIAN_POINT ( 'NONE',  ( 10.00000000000000000, 49.76630880786309064, 26.49895292618021614 ) ) ;
#17613 = AXIS2_PLACEMENT_3D ( 'NONE', #3038, #2932, #14836 ) ;
#17614 = EDGE_CURVE ( 'NONE', #11942, #607, #5840, .T. ) ;
#17615 = DIRECTION ( 'NONE',  ( 0.000000000000000000, 0.000000000000000000, 1.000000000000000000 ) ) ;
#17616 = DIRECTION ( 'NONE',  ( 0.000000000000000000, 1.000000000000000000, 0.000000000000000000 ) ) ;
#17617 = CARTESIAN_POINT ( 'NONE',  ( 0.000000000000000000, -30.00000000000000000, 0.000000000000000000 ) ) ;
#17618 = ORIENTED_EDGE ( 'NONE', *, *, #1609, .F. ) ;
#17619 = CARTESIAN_POINT ( 'NONE',  ( 11.25000000000000000, 3.429011037612589670E-15, 28.00000000000000355 ) ) ;
#17620 = CARTESIAN_POINT ( 'NONE',  ( 10.00000000000000000, 25.42247726998032320, -12.18267823974723640 ) ) ;
#17621 = EDGE_LOOP ( 'NONE', ( #14603, #2198, #7311, #8790 ) ) ;
#17622 = CARTESIAN_POINT ( 'NONE',  ( 0.000000000000000000, 0.000000000000000000, 0.000000000000000000 ) ) ;
#17623 = DIRECTION ( 'NONE',  ( -1.000000000000000000, -0.000000000000000000, -0.000000000000000000 ) ) ;
#17624 = ADVANCED_FACE ( 'NONE', ( #13146 ), #7513, .T. ) ;
#17625 = EDGE_CURVE ( 'NONE', #3888, #17281, #14664, .T. ) ;
#17626 = AXIS2_PLACEMENT_3D ( 'NONE', #3235, #1615, #3341 ) ;
#17627 = AXIS2_PLACEMENT_3D ( 'NONE', #10967, #17935, #16884 ) ;
#17628 = ADVANCED_FACE ( 'NONE', ( #14746 ), #4294, .T. ) ;
#17629 = EDGE_CURVE ( 'NONE', #8275, #17362, #11025, .T. ) ;
#17630 = ORIENTED_EDGE ( 'NONE', *, *, #12136, .T. ) ;
#17631 = DIRECTION ( 'NONE',  ( -1.000000000000000000, -0.000000000000000000, -0.000000000000000000 ) ) ;
#17632 = DIRECTION ( 'NONE',  ( 0.000000000000000000, 0.000000000000000000, 1.000000000000000000 ) ) ;
#17633 = ORIENTED_EDGE ( 'NONE', *, *, #5026, .F. ) ;
#17634 = SURFACE_SIDE_STYLE ('',( #1997 ) ) ;
#17635 = CARTESIAN_POINT ( 'NONE',  ( 10.00000000000000000, 25.38428207620331634, -6.681932690256706664 ) ) ;
#17636 = EDGE_CURVE ( 'NONE', #2561, #16544, #10130, .T. ) ;
#17637 = CARTESIAN_POINT ( 'NONE',  ( 10.00000000000000000, -50.71018745830461683, 24.33982105418882469 ) ) ;
#17638 = CIRCLE ( 'NONE', #1223, 33.00000000003299760 ) ;
#17639 = LINE ( 'NONE', #16488, #1577 ) ;
#17640 = DIRECTION ( 'NONE',  ( -1.000000000000000000, 0.000000000000000000, -0.000000000000000000 ) ) ;
#17641 = VERTEX_POINT ( 'NONE', #17703 ) ;
#17642 = DIRECTION ( 'NONE',  ( 0.000000000000000000, 0.000000000000000000, 1.000000000000000000 ) ) ;
#17643 = ORIENTED_EDGE ( 'NONE', *, *, #12889, .T. ) ;
#17644 =( LENGTH_UNIT ( ) NAMED_UNIT ( * ) SI_UNIT ( .MILLI., .METRE. ) );
#17645 = CARTESIAN_POINT ( 'NONE',  ( 0.000000000000000000, 0.000000000000000000, -5.000000000000000888 ) ) ;
#17646 = ORIENTED_EDGE ( 'NONE', *, *, #14936, .T. ) ;
#17647 = ADVANCED_FACE ( 'NONE', ( #7327 ), #101, .T. ) ;
#17648 = CONTEXT_DEPENDENT_SHAPE_REPRESENTATION ( #17777, #16058 ) ;
#17649 = EDGE_LOOP ( 'NONE', ( #7026, #17052 ) ) ;
#17650 = ORIENTED_EDGE ( 'NONE', *, *, #18677, .T. ) ;
#17651 = AXIS2_PLACEMENT_3D ( 'NONE', #135, #5929, #11751 ) ;
#17652 = APPLICATION_CONTEXT ( 'automotive_design' ) ;
#17653 = EDGE_CURVE ( 'NONE', #4800, #701, #5898, .T. ) ;
#17654 =( GEOMETRIC_REPRESENTATION_CONTEXT ( 3 ) GLOBAL_UNCERTAINTY_ASSIGNED_CONTEXT ( ( #632 ) ) GLOBAL_UNIT_ASSIGNED_CONTEXT ( ( #16986, #9737, #12787 ) ) REPRESENTATION_CONTEXT ( 'NONE', 'WORKASPACE' ) );
#17655 = DIRECTION ( 'NONE',  ( 0.000000000000000000, 0.000000000000000000, 1.000000000000000000 ) ) ;
#17656 = CARTESIAN_POINT ( 'NONE',  ( 10.00000000000000000, 0.000000000000000000, 0.000000000000000000 ) ) ;
#17657 = CARTESIAN_POINT ( 'NONE',  ( -10.00000000000000000, 0.000000000000000000, 0.000000000000000000 ) ) ;
#17658 = CARTESIAN_POINT ( 'NONE',  ( -79.64793068852898728, -30.00000000000000000, -31.86039329588756530 ) ) ;
#17659 = CARTESIAN_POINT ( 'NONE',  ( 10.00000000000000000, 38.81885513159988932, 40.70683587897971734 ) ) ;
#17660 = CARTESIAN_POINT ( 'NONE',  ( -56.50000000009000445, -30.00000000000000000, 2.650000000000374278 ) ) ;
#17661 = DIRECTION ( 'NONE',  ( -1.000000000000000000, -0.000000000000000000, 0.000000000000000000 ) ) ;
#17662 = CARTESIAN_POINT ( 'NONE',  ( 1.999999999999998224, -3.464101615137772594, -3.142992957459239012 ) ) ;
#17663 = ORIENTED_EDGE ( 'NONE', *, *, #6249, .F. ) ;
#17664 = CARTESIAN_POINT ( 'NONE',  ( -90.00000000009003998, 1.821459649775647449E-14, -5.746271514173173500E-15 ) ) ;
#17665 = CYLINDRICAL_SURFACE ( 'NONE', #14409, 26.24900000002624978 ) ;
#17666 = DIRECTION ( 'NONE',  ( -1.000000000000000000, -0.000000000000000000, -0.000000000000000000 ) ) ;
#17667 = VERTEX_POINT ( 'NONE', #3510 ) ;
#17668 = ORIENTED_EDGE ( 'NONE', *, *, #10170, .T. ) ;
#17669 = FACE_OUTER_BOUND ( 'NONE', #5092, .T. ) ;
#17670 = VECTOR ( 'NONE', #4860, 999.9999999999998863 ) ;
#17671 = CARTESIAN_POINT ( 'NONE',  ( 0.000000000000000000, 11.24999999999999467, 0.000000000000000000 ) ) ;
#17672 = ORIENTED_EDGE ( 'NONE', *, *, #996, .T. ) ;
#17673 = ADVANCED_FACE ( 'NONE', ( #7610, #16553, #9505, #3422, #13427, #9216, #9414 ), #15319, .F. ) ;
#17674 = CARTESIAN_POINT ( 'NONE',  ( 0.000000000000000000, 58.55669782892493203, -23.24033432160376478 ) ) ;
#17675 = CARTESIAN_POINT ( 'NONE',  ( 0.6640947660595348800, -4.471078309994175548, -3.602146406945708090 ) ) ;
#17676 = CARTESIAN_POINT ( 'NONE',  ( 4.999999999999999112, -61.03368945066424800, -15.61693798565561409 ) ) ;
#17677 = ORIENTED_EDGE ( 'NONE', *, *, #16808, .F. ) ;
#17679 = AXIS2_PLACEMENT_3D ( 'NONE', #12048, #13492, #16441 ) ;
#17678 = CARTESIAN_POINT ( 'NONE',  ( -2.688821387764050996E-14, -4.618802153517012954, -0.4999999999999995559 ) ) ;
#17680 = ORIENTED_EDGE ( 'NONE', *, *, #3460, .T. ) ;
#17681 = CARTESIAN_POINT ( 'NONE',  ( -10.00000000000000000, 0.000000000000000000, 0.000000000000000000 ) ) ;
#17682 = VERTEX_POINT ( 'NONE', #9309 ) ;
#17683 = DIRECTION ( 'NONE',  ( -1.000000000000000000, 0.000000000000000000, -0.000000000000000000 ) ) ;
#17684 = FACE_OUTER_BOUND ( 'NONE', #4718, .T. ) ;
#17685 = ORIENTED_EDGE ( 'NONE', *, *, #18679, .F. ) ;
#17686 = VERTEX_POINT ( 'NONE', #6175 ) ;
#17687 = ADVANCED_FACE ( 'NONE', ( #18075 ), #564, .T. ) ;
#17688 = DIRECTION ( 'NONE',  ( -1.000000000000000000, 0.000000000000000000, 0.000000000000000000 ) ) ;
#17689 = ORIENTED_EDGE ( 'NONE', *, *, #2408, .T. ) ;
#17690 = FACE_OUTER_BOUND ( 'NONE', #2577, .T. ) ;
#17691 = CIRCLE ( 'NONE', #9475, 63.00000000006298961 ) ;
#17692 = EDGE_CURVE ( 'NONE', #4897, #13691, #3616, .T. ) ;
#17693 = DIRECTION ( 'NONE',  ( -1.000000000000000000, -0.000000000000000000, 0.000000000000000000 ) ) ;
#17694 = VECTOR ( 'NONE', #11410, 999.9999999999997726 ) ;
#17695 = ORIENTED_EDGE ( 'NONE', *, *, #4579, .T. ) ;
#17696 = ORIENTED_EDGE ( 'NONE', *, *, #3498, .T. ) ;
#17697 = DIRECTION ( 'NONE',  ( -1.000000000000000000, -0.000000000000000000, -0.000000000000000000 ) ) ;
#17698 = DIRECTION ( 'NONE',  ( -1.000000000000000000, 0.000000000000000000, -0.000000000000000000 ) ) ;
#17699 = DIRECTION ( 'NONE',  ( -0.000000000000000000, 1.000000000000000000, -0.000000000000000000 ) ) ;
#17700 = ORIENTED_EDGE ( 'NONE', *, *, #15979, .T. ) ;
#17701 = CARTESIAN_POINT ( 'NONE',  ( 0.000000000000000000, -5.117658387065794099E-13, -47.64999999999999858 ) ) ;
#17702 = DIRECTION ( 'NONE',  ( 1.000000000000000000, -3.469446951953611231E-16, 0.000000000000000000 ) ) ;
#17703 = CARTESIAN_POINT ( 'NONE',  ( 0.9999999999999997780, -27.60846790388774608, 0.000000000000000000 ) ) ;
#17704 = DIRECTION ( 'NONE',  ( 0.000000000000000000, 0.000000000000000000, -1.000000000000000000 ) ) ;
#17705 = ORIENTED_EDGE ( 'NONE', *, *, #8192, .T. ) ;
#17706 = DIRECTION ( 'NONE',  ( 0.000000000000000000, 0.000000000000000000, 1.000000000000000000 ) ) ;
#17707 = DIRECTION ( 'NONE',  ( 0.000000000000000000, 0.000000000000000000, 1.000000000000000000 ) ) ;
#17708 = CIRCLE ( 'NONE', #14369, 26.24900000002624978 ) ;
#17709 = EDGE_LOOP ( 'NONE', ( #2462, #7244, #11436, #16958 ) ) ;
#17710 = DIRECTION ( 'NONE',  ( -1.000000000000000000, 0.000000000000000000, 0.000000000000000000 ) ) ;
#17711 = DIRECTION ( 'NONE',  ( -1.000000000000000000, 0.000000000000000000, 0.000000000000000000 ) ) ;
#17712 = VERTEX_POINT ( 'NONE', #17791 ) ;
#17713 = AXIS2_PLACEMENT_3D ( 'NONE', #7396, #13212, #1403 ) ;
#17714 = DIRECTION ( 'NONE',  ( -1.000000000000000000, 0.000000000000000000, -0.000000000000000000 ) ) ;
#17715 = AXIS2_PLACEMENT_3D ( 'NONE', #8406, #18221, #6601 ) ;
#17716 = ORIENTED_EDGE ( 'NONE', *, *, #1273, .F. ) ;
#17717 = DIRECTION ( 'NONE',  ( 1.000000000000000000, 0.000000000000000000, 0.000000000000000000 ) ) ;
#17718 = EDGE_CURVE ( 'NONE', #10053, #7713, #16816, .T. ) ;
#17719 = DIRECTION ( 'NONE',  ( -1.000000000000000000, -0.000000000000000000, -0.000000000000000000 ) ) ;
#17720 = ADVANCED_FACE ( 'NONE', ( #13515 ), #4745, .T. ) ;
#17721 = ADVANCED_FACE ( 'NONE', ( #10739 ), #15036, .T. ) ;
#17722 = DIRECTION ( 'NONE',  ( -1.000000000000000000, -0.000000000000000000, -0.000000000000000000 ) ) ;
#17723 = LINE ( 'NONE', #1629, #7342 ) ;
#17724 = CARTESIAN_POINT ( 'NONE',  ( 0.2500000000000002220, 0.000000000000000000, 0.000000000000000000 ) ) ;
#17725 = EDGE_LOOP ( 'NONE', ( #1915, #9690, #17919, #18404 ) ) ;
#17726 = CARTESIAN_POINT ( 'NONE',  ( 10.00000000000000000, -45.00825343884996954, -33.95787273855293620 ) ) ;
#17727 = EDGE_LOOP ( 'NONE', ( #9416, #13038 ) ) ;
#17728 = EDGE_CURVE ( 'NONE', #15674, #2059, #16378, .T. ) ;
#17729 = DIRECTION ( 'NONE',  ( 0.000000000000000000, 0.3090169943749411785, 0.9510565162951556406 ) ) ;
#17730 = ORIENTED_EDGE ( 'NONE', *, *, #12009, .F. ) ;
#17731 = CONTEXT_DEPENDENT_SHAPE_REPRESENTATION ( #7798, #397 ) ;
#17732 = AXIS2_PLACEMENT_3D ( 'NONE', #2836, #8637, #13032 ) ;
#17733 = VERTEX_POINT ( 'NONE', #9132 ) ;
#17734 = CLOSED_SHELL ( 'NONE', ( #12819, #7290, #10917, #2079, #11578, #16746, #5028, #13977, #11675, #2494, #2846, #17273, #9328, #12920, #9327, #9944, #6215, #7608, #8766, #3513, #10772, #2099, #1919, #8825, #1447, #4762, #9681, #5417, #9355, #10994 ) ) ;
#17735 = VERTEX_POINT ( 'NONE', #7787 ) ;
#17736 = EDGE_CURVE ( 'NONE', #2243, #14680, #11938, .T. ) ;
#17737 = EDGE_LOOP ( 'NONE', ( #18765, #14455, #5409, #5136 ) ) ;
#17738 = DIRECTION ( 'NONE',  ( 0.000000000000000000, 1.000000000000000000, 0.000000000000000000 ) ) ;
#17739 = DIRECTION ( 'NONE',  ( -1.000000000000000000, -0.000000000000000000, 0.000000000000000000 ) ) ;
#17740 = DIRECTION ( 'NONE',  ( -1.000000000000000000, -0.000000000000000000, 0.000000000000000000 ) ) ;
#17741 = DIRECTION ( 'NONE',  ( 0.000000000000000000, 0.000000000000000000, 1.000000000000000000 ) ) ;
#17742 = ADVANCED_FACE ( 'NONE', ( #13617 ), #17987, .F. ) ;
#17743 = CIRCLE ( 'NONE', #11057, 4.000000000000000000 ) ;
#17744 = CARTESIAN_POINT ( 'NONE',  ( 5.000000000000000000, 23.24033432160521784, -58.55669782892436359 ) ) ;
#17745 = CARTESIAN_POINT ( 'NONE',  ( -79.64793068852898728, -34.99999999999999289, -29.21039329588757383 ) ) ;
#17746 = LINE ( 'NONE', #1933, #5640 ) ;
#17747 = DIRECTION ( 'NONE',  ( -0.000000000000000000, -0.000000000000000000, 1.000000000000000000 ) ) ;
#17748 = ORIENTED_EDGE ( 'NONE', *, *, #476, .T. ) ;
#17749 =( LENGTH_UNIT ( ) NAMED_UNIT ( * ) SI_UNIT ( .MILLI., .METRE. ) );
#17750 = CARTESIAN_POINT ( 'NONE',  ( 3.510273485745307731, 2.827716139362654424, -3.610536846335885564 ) ) ;
#17751 = DIRECTION ( 'NONE',  ( -1.000000000000000000, -0.000000000000000000, -0.000000000000000000 ) ) ;
#17752 = ORIENTED_EDGE ( 'NONE', *, *, #18570, .F. ) ;
#17753 = ORIENTED_EDGE ( 'NONE', *, *, #11723, .F. ) ;
#17754 = EDGE_CURVE ( 'NONE', #18379, #5754, #13710, .T. ) ;
#17755 = CARTESIAN_POINT ( 'NONE',  ( -2.687328764639638656, 3.067272167851286202, -0.05923475698270370959 ) ) ;
#17756 = DIRECTION ( 'NONE',  ( 6.123233995736766036E-17, -1.000000000000000000, 0.000000000000000000 ) ) ;
#17757 = DIRECTION ( 'NONE',  ( 0.000000000000000000, 0.000000000000000000, 1.000000000000000000 ) ) ;
#17758 = ORIENTED_EDGE ( 'NONE', *, *, #9627, .T. ) ;
#17759 = DIRECTION ( 'NONE',  ( 1.000000000000000000, -0.000000000000000000, -0.000000000000000000 ) ) ;
#17760 = DIRECTION ( 'NONE',  ( 1.000000000000000000, 0.000000000000000000, 0.000000000000000000 ) ) ;
#17761 = DIRECTION ( 'NONE',  ( 1.000000000000000000, 0.000000000000000000, 0.000000000000000000 ) ) ;
#17762 = ORIENTED_EDGE ( 'NONE', *, *, #12078, .F. ) ;
#17763 = DIRECTION ( 'NONE',  ( -1.000000000000000000, -0.000000000000000000, -0.000000000000000000 ) ) ;
#17764 = ORIENTED_EDGE ( 'NONE', *, *, #12721, .T. ) ;
#17765 = UNCERTAINTY_MEASURE_WITH_UNIT (LENGTH_MEASURE( 1.000000000000000082E-05 ), #7673, 'distance_accuracy_value', 'NONE');
#17766 = CARTESIAN_POINT ( 'NONE',  ( 0.000000000000000000, -14.19907017806883864, 22.07705612348834734 ) ) ;
#17767 = VERTEX_POINT ( 'NONE', #460 ) ;
#17768 = DIRECTION ( 'NONE',  ( -0.000000000000000000, -1.000000000000000000, -0.000000000000000000 ) ) ;
#17769 = CARTESIAN_POINT ( 'NONE',  ( -4.175648173966055587, 2.207990556236529844, -3.469390959564062626 ) ) ;
#17770 = EDGE_LOOP ( 'NONE', ( #3797, #14104, #13543, #12071 ) ) ;
#17771 = VERTEX_POINT ( 'NONE', #18174 ) ;
#17772 = ADVANCED_FACE ( 'NONE', ( #6463 ), #12269, .T. ) ;
#17773 = CARTESIAN_POINT ( 'NONE',  ( 10.00000000000000000, 0.000000000000000000, 56.24900000005625600 ) ) ;
#17774 =( NAMED_UNIT ( * ) SI_UNIT ( $, .STERADIAN. ) SOLID_ANGLE_UNIT ( ) );
#17775 = ORIENTED_EDGE ( 'NONE', *, *, #2996, .F. ) ;
#17776 = CARTESIAN_POINT ( 'NONE',  ( 0.000000000000000000, -32.46095361140688595, -5.940243314904558147 ) ) ;
#17777 =( REPRESENTATION_RELATIONSHIP ('NONE','NONE', #11014, #11521 ) REPRESENTATION_RELATIONSHIP_WITH_TRANSFORMATION ( #10482 )SHAPE_REPRESENTATION_RELATIONSHIP( ) );
#17778 = DIRECTION ( 'NONE',  ( -1.000000000000000000, -0.000000000000000000, -0.000000000000000000 ) ) ;
#17779 = VECTOR ( 'NONE', #18582, 1000.000000000000000 ) ;
#17780 = AXIS2_PLACEMENT_3D ( 'NONE', #8839, #183, #6262 ) ;
#17781 = ORIENTED_EDGE ( 'NONE', *, *, #18266, .F. ) ;
#17782 = EDGE_CURVE ( 'NONE', #9002, #14729, #15286, .T. ) ;
#17783 = ORIENTED_EDGE ( 'NONE', *, *, #13544, .F. ) ;
#17784 = CARTESIAN_POINT ( 'NONE',  ( 1.250000000000000000, -6.429618962271402616, -1.000000000000000000 ) ) ;
#17785 = CARTESIAN_POINT ( 'NONE',  ( 0.000000000000000000, 15.00000000000000000, 0.000000000000000000 ) ) ;
#17786 = CARTESIAN_POINT ( 'NONE',  ( 0.000000000000000000, -26.45033635316118747, 36.40576474687271258 ) ) ;
#17787 = ORIENTED_EDGE ( 'NONE', *, *, #8474, .F. ) ;
#17788 = CARTESIAN_POINT ( 'NONE',  ( 1.411581201560190495E-15, 4.862606272033091592, -3.745885042887436622 ) ) ;
#17789 = ADVANCED_FACE ( 'NONE', ( #10932 ), #16756, .T. ) ;
#17790 = CARTESIAN_POINT ( 'NONE',  ( 10.04305231718605285, -26.50000000000000000, -28.25933677959240597 ) ) ;
#17791 = CARTESIAN_POINT ( 'NONE',  ( 0.000000000000000000, -34.13306034420152457, -44.70888270294198463 ) ) ;
#17792 = CARTESIAN_POINT ( 'NONE',  ( 0.000000000000000000, 18.38754094778241210, 53.29895248911682870 ) ) ;
#17793 = VERTEX_POINT ( 'NONE', #12649 ) ;
#17794 = DIRECTION ( 'NONE',  ( 0.000000000000000000, 0.8910065241883656784, 0.4539904997395510788 ) ) ;
#17795 = CARTESIAN_POINT ( 'NONE',  ( 0.000000000000000000, -53.06836994729219725, -18.64666490672428623 ) ) ;
#17796 = LINE ( 'NONE', #14509, #3846 ) ;
#17797 = ORIENTED_EDGE ( 'NONE', *, *, #14074, .F. ) ;
#17798 = DIRECTION ( 'NONE',  ( 0.000000000000000000, 0.000000000000000000, 1.000000000000000000 ) ) ;
#17799 = DIRECTION ( 'NONE',  ( -1.000000000000000000, -0.000000000000000000, 0.000000000000000000 ) ) ;
#17800 = AXIS2_PLACEMENT_3D ( 'NONE', #18160, #15499, #9779 ) ;
#17801 = AXIS2_PLACEMENT_3D ( 'NONE', #11310, #12646, #2261 ) ;
#17802 = AXIS2_PLACEMENT_3D ( 'NONE', #15299, #7963, #3689 ) ;
#17803 = ORIENTED_EDGE ( 'NONE', *, *, #15700, .F. ) ;
#17804 = SURFACE_STYLE_FILL_AREA ( #9585 ) ;
#17805 = CIRCLE ( 'NONE', #11427, 56.24900000005627021 ) ;
#17806 = ORIENTED_EDGE ( 'NONE', *, *, #2583, .T. ) ;
#17807 = DIRECTION ( 'NONE',  ( 0.000000000000000000, 0.000000000000000000, 1.000000000000000000 ) ) ;
#17808 = AXIS2_PLACEMENT_3D ( 'NONE', #17450, #5914, #5830 ) ;
#17809 = CARTESIAN_POINT ( 'NONE',  ( -0.3789929286210603765, 13.24999999999999822, 24.99712712213256438 ) ) ;
#17810 = CARTESIAN_POINT ( 'NONE',  ( 10.00000000000000000, 0.000000000000000000, 0.000000000000000000 ) ) ;
#17811 = CARTESIAN_POINT ( 'NONE',  ( 45.00000000000000000, 0.000000000000000000, -5.120903701083534543E-13 ) ) ;
#17812 = DIRECTION ( 'NONE',  ( -1.000000000000000000, -0.000000000000000000, -0.000000000000000000 ) ) ;
#17813 = ORIENTED_EDGE ( 'NONE', *, *, #10514, .T. ) ;
#17814 = CARTESIAN_POINT ( 'NONE',  ( 10.04305231718605285, -30.00000000000000000, -33.55933677959240669 ) ) ;
#17815 = ORIENTED_EDGE ( 'NONE', *, *, #12861, .T. ) ;
#17816 = CARTESIAN_POINT ( 'NONE',  ( -26.29305231718584324, -26.50000000000000000, 19.10302069950530779 ) ) ;
#17817 = ORIENTED_EDGE ( 'NONE', *, *, #17499, .T. ) ;
#17818 = VECTOR ( 'NONE', #4047, 1000.000000000000000 ) ;
#17819 = AXIS2_PLACEMENT_3D ( 'NONE', #3569, #3929, #17943 ) ;
#17820 = EDGE_CURVE ( 'NONE', #5675, #3305, #13474, .T. ) ;
#17821 = VERTEX_POINT ( 'NONE', #14079 ) ;
#17822 = CIRCLE ( 'NONE', #6868, 12.00000000001200817 ) ;
#17823 = AXIS2_PLACEMENT_3D ( 'NONE', #7761, #17683, #8914 ) ;
#17824 = CIRCLE ( 'NONE', #10524, 2.649999999999992806 ) ;
#17825 = EDGE_CURVE ( 'NONE', #13818, #6354, #14670, .T. ) ;
#17826 = ADVANCED_FACE ( 'NONE', ( #12554, #5601, #6941 ), #5422, .F. ) ;
#17827 = VERTEX_POINT ( 'NONE', #15417 ) ;
#17828 = ORIENTED_EDGE ( 'NONE', *, *, #896, .F. ) ;
#17829 = DIRECTION ( 'NONE',  ( 0.000000000000000000, 0.000000000000000000, -1.000000000000000000 ) ) ;
#17830 = EDGE_CURVE ( 'NONE', #10460, #7525, #17417, .T. ) ;
#17831 = PRESENTATION_STYLE_ASSIGNMENT (( #15178 ) ) ;
#17832 = CIRCLE ( 'NONE', #14785, 30.00000000000000000 ) ;
#17833 = DIRECTION ( 'NONE',  ( 1.000000000000000000, 0.000000000000000000, 0.000000000000000000 ) ) ;
#17834 = DIRECTION ( 'NONE',  ( -1.000000000000000000, 0.000000000000000000, 0.000000000000000000 ) ) ;
#17835 = ADVANCED_FACE ( 'NONE', ( #13991 ), #8078, .T. ) ;
#17836 = CIRCLE ( 'NONE', #11769, 24.00000000002399858 ) ;
#17837 = PLANE ( 'NONE',  #14511 ) ;
#17838 = DIRECTION ( 'NONE',  ( 0.000000000000000000, 0.000000000000000000, 1.000000000000000000 ) ) ;
#17839 = CIRCLE ( 'NONE', #7194, 24.00000000002399858 ) ;
#17840 = DIRECTION ( 'NONE',  ( -1.000000000000000000, 0.000000000000000000, -0.000000000000000000 ) ) ;
#17841 = AXIS2_PLACEMENT_3D ( 'NONE', #8479, #13051, #14462 ) ;
#17842 = CARTESIAN_POINT ( 'NONE',  ( 10.00000000000000000, -42.79754323328189969, -11.25576474687263229 ) ) ;
#17843 = ORIENTED_EDGE ( 'NONE', *, *, #11679, .F. ) ;
#17844 = DIRECTION ( 'NONE',  ( 0.000000000000000000, 0.000000000000000000, 1.000000000000000000 ) ) ;
#17845 = EDGE_CURVE ( 'NONE', #16942, #7722, #5245, .T. ) ;
#17846 = DIRECTION ( 'NONE',  ( 0.000000000000000000, 0.000000000000000000, 1.000000000000000000 ) ) ;
#17847 = DIRECTION ( 'NONE',  ( 0.000000000000000000, 0.000000000000000000, 1.000000000000000000 ) ) ;
#17848 = ORIENTED_EDGE ( 'NONE', *, *, #11481, .T. ) ;
#17849 = ORIENTED_EDGE ( 'NONE', *, *, #17508, .F. ) ;
#17850 = CARTESIAN_POINT ( 'NONE',  ( 0.000000000000000000, 0.000000000000000000, 0.000000000000000000 ) ) ;
#17851 = DIRECTION ( 'NONE',  ( 1.000000000000000000, 0.000000000000000000, 0.000000000000000000 ) ) ;
#17852 = CARTESIAN_POINT ( 'NONE',  ( -11.15000000000000391, 0.000000000000000000, 30.00000000000000711 ) ) ;
#17853 = ORIENTED_EDGE ( 'NONE', *, *, #12752, .T. ) ;
#17854 = VECTOR ( 'NONE', #14191, 1000.000000000000000 ) ;
#17855 = ADVANCED_FACE ( 'NONE', ( #9699 ), #5309, .T. ) ;
#17856 = CIRCLE ( 'NONE', #11492, 27.50000000000000000 ) ;
#17857 = EDGE_CURVE ( 'NONE', #6557, #12264, #2551, .T. ) ;
#17858 = AXIS2_PLACEMENT_3D ( 'NONE', #11724, #1714, #18063 ) ;
#17859 = VECTOR ( 'NONE', #8457, 1000.000000000000227 ) ;
#17860 = CARTESIAN_POINT ( 'NONE',  ( 10.00000000000000000, 55.83748330407408389, -7.813799127873475747 ) ) ;
#17861 = ADVANCED_FACE ( 'NONE', ( #9884 ), #16946, .T. ) ;
#17862 = DIRECTION ( 'NONE',  ( -1.000000000000000000, 0.000000000000000000, 0.000000000000000000 ) ) ;
#17863 = CARTESIAN_POINT ( 'NONE',  ( 0.000000000000000000, 0.000000000000000000, 0.000000000000000000 ) ) ;
#17864 = ADVANCED_FACE ( 'NONE', ( #1039 ), #5217, .F. ) ;
#17865 = ORIENTED_EDGE ( 'NONE', *, *, #5986, .F. ) ;
#17866 = CARTESIAN_POINT ( 'NONE',  ( 10.00000000000000000, 0.000000000000000000, 0.000000000000000000 ) ) ;
#17867 = AXIS2_PLACEMENT_3D ( 'NONE', #5351, #6875, #7227 ) ;
#17868 = ORIENTED_EDGE ( 'NONE', *, *, #6779, .T. ) ;
#17869 = CARTESIAN_POINT ( 'NONE',  ( -31.74999999999995737, 0.000000000000000000, 0.000000000000000000 ) ) ;
#17870 = EDGE_LOOP ( 'NONE', ( #301, #14149, #16649, #15042 ) ) ;
#17871 = AXIS2_PLACEMENT_3D ( 'NONE', #12599, #3749, #9548 ) ;
#17872 = FACE_OUTER_BOUND ( 'NONE', #9849, .T. ) ;
#17873 = FACE_OUTER_BOUND ( 'NONE', #7715, .T. ) ;
#17874 = AXIS2_PLACEMENT_3D ( 'NONE', #3022, #18725, #2737 ) ;
#17875 = ORIENTED_EDGE ( 'NONE', *, *, #13687, .T. ) ;
#17876 = ORIENTED_EDGE ( 'NONE', *, *, #1783, .T. ) ;
#17877 = LINE ( 'NONE', #4547, #6594 ) ;
#17878 = ORIENTED_EDGE ( 'NONE', *, *, #17625, .T. ) ;
#17879 = DIRECTION ( 'NONE',  ( -0.8191520442889902442, 0.000000000000000000, -0.5735764363510482688 ) ) ;
#17880 = AXIS2_PLACEMENT_3D ( 'NONE', #17405, #9976, #9877 ) ;
#17881 = CIRCLE ( 'NONE', #4216, 24.00000000002400569 ) ;
#17882 = DIRECTION ( 'NONE',  ( -0.000000000000000000, 1.000000000000000000, -0.000000000000000000 ) ) ;
#17883 = VECTOR ( 'NONE', #8609, 1000.000000000000000 ) ;
#17884 = VECTOR ( 'NONE', #5443, 1000.000000000000000 ) ;
#17885 = EDGE_CURVE ( 'NONE', #2652, #2958, #88, .T. ) ;
#17886 = ORIENTED_EDGE ( 'NONE', *, *, #13104, .F. ) ;
#17887 = PRODUCT ( 'motor', 'motor', '', ( #15848 ) ) ;
#17888 = ORIENTED_EDGE ( 'NONE', *, *, #13067, .F. ) ;
#17889 = CARTESIAN_POINT ( 'NONE',  ( 10.00000000000000000, 7.478235706488965739, 55.74967257055886449 ) ) ;
#17890 = CARTESIAN_POINT ( 'NONE',  ( 10.00000000000000000, 32.11449294037269198, -54.20017844242477878 ) ) ;
#17891 = DIRECTION ( 'NONE',  ( -1.000000000000000000, 0.000000000000000000, 0.000000000000000000 ) ) ;
#17892 = ORIENTED_EDGE ( 'NONE', *, *, #7543, .F. ) ;
#17893 = CARTESIAN_POINT ( 'NONE',  ( 0.4999999999999916733, -30.39588787977742257, -2.000000000000000000 ) ) ;
#17894 = CARTESIAN_POINT ( 'NONE',  ( 2.449293598294706513E-15, -30.00000000000000000, -20.00000000000000000 ) ) ;
#17895 = CARTESIAN_POINT ( 'NONE',  ( 10.00000000000000000, 9.823366686500662581, 55.51919907100656104 ) ) ;
#17896 = CIRCLE ( 'NONE', #2994, 33.00000000003299760 ) ;
#17897 = CARTESIAN_POINT ( 'NONE',  ( 2.500000000000000000, 2.357898499370431722, -2.818925648462311528E-15 ) ) ;
#17898 = EDGE_LOOP ( 'NONE', ( #16948, #7680, #4428, #13785 ) ) ;
#17899 = CARTESIAN_POINT ( 'NONE',  ( 0.000000000000000000, -24.46385708179990459, 9.514709542736804693 ) ) ;
#17900 = AXIS2_PLACEMENT_3D ( 'NONE', #2962, #6182, #377 ) ;
#17901 = EDGE_LOOP ( 'NONE', ( #8997, #11615 ) ) ;
#17902 = DIRECTION ( 'NONE',  ( 0.000000000000000000, -1.000000000000000000, 1.287488025362403787E-15 ) ) ;
#17903 = DIRECTION ( 'NONE',  ( 0.000000000000000000, 0.000000000000000000, 1.000000000000000000 ) ) ;
#17904 = MECHANICAL_DESIGN_GEOMETRIC_PRESENTATION_REPRESENTATION (  '', ( #13042 ), #11538 ) ;
#17905 = AXIS2_PLACEMENT_3D ( 'NONE', #3706, #6746, #8077 ) ;
#17906 = VECTOR ( 'NONE', #9545, 1000.000000000000000 ) ;
#17907 = EDGE_CURVE ( 'NONE', #15674, #15225, #14172, .T. ) ;
#17908 = ORIENTED_EDGE ( 'NONE', *, *, #4052, .F. ) ;
#17909 = VECTOR ( 'NONE', #8187, 1000.000000000000000 ) ;
#17910 = LINE ( 'NONE', #6824, #17670 ) ;
#17911 = AXIS2_PLACEMENT_3D ( 'NONE', #13443, #17717, #10667 ) ;
#17912 = ORIENTED_EDGE ( 'NONE', *, *, #12267, .T. ) ;
#17913 = AXIS2_PLACEMENT_3D ( 'NONE', #5600, #2749, #4442 ) ;
#17914 = CARTESIAN_POINT ( 'NONE',  ( -31.74999999999995737, 0.000000000000000000, 0.000000000000000000 ) ) ;
#17915 = DIRECTION ( 'NONE',  ( -1.000000000000000000, 0.000000000000000000, 0.000000000000000000 ) ) ;
#17916 = CARTESIAN_POINT ( 'NONE',  ( -4.799999999999999822, 5.878304635907294211E-16, 0.000000000000000000 ) ) ;
#17917 = DIRECTION ( 'NONE',  ( 0.000000000000000000, 0.000000000000000000, 1.000000000000000000 ) ) ;
#17918 = DIRECTION ( 'NONE',  ( 0.000000000000000000, -0.8090169943749531134, 0.5877852522924653655 ) ) ;
#17919 = ORIENTED_EDGE ( 'NONE', *, *, #14169, .T. ) ;
#17920 = DIRECTION ( 'NONE',  ( 0.000000000000000000, 0.000000000000000000, 1.000000000000000000 ) ) ;
#17921 = CARTESIAN_POINT ( 'NONE',  ( 0.000000000000000000, 27.94286728106393269, 15.73043801031642808 ) ) ;
#17922 = VECTOR ( 'NONE', #11999, 1000.000000000000000 ) ;
#17923 = ORIENTED_EDGE ( 'NONE', *, *, #11370, .T. ) ;
#17924 = ADVANCED_FACE ( 'NONE', ( #2650 ), #1138, .T. ) ;
#17925 = VECTOR ( 'NONE', #16558, 1000.000000000000000 ) ;
#17926 = ORIENTED_EDGE ( 'NONE', *, *, #1120, .T. ) ;
#17927 = ADVANCED_FACE ( 'NONE', ( #14280 ), #1236, .F. ) ;
#17928 = VERTEX_POINT ( 'NONE', #4543 ) ;
#17929 = ORIENTED_EDGE ( 'NONE', *, *, #10814, .T. ) ;
#17930 = DIRECTION ( 'NONE',  ( 0.000000000000000000, 0.000000000000000000, 1.000000000000000000 ) ) ;
#17931 = DIRECTION ( 'NONE',  ( 0.000000000000000000, 0.000000000000000000, 1.000000000000000000 ) ) ;
#17932 = DIRECTION ( 'NONE',  ( -1.000000000000000000, -0.000000000000000000, -0.000000000000000000 ) ) ;
#17933 = DIRECTION ( 'NONE',  ( -1.000000000000000000, 0.000000000000000000, -0.000000000000000000 ) ) ;
#17934 = VECTOR ( 'NONE', #17206, 1000.000000000000000 ) ;
#17935 = DIRECTION ( 'NONE',  ( -1.000000000000000000, 0.000000000000000000, -0.000000000000000000 ) ) ;
#17936 = PLANE ( 'NONE',  #9975 ) ;
#17937 = DIRECTION ( 'NONE',  ( -1.000000000000000000, -0.000000000000000000, -0.000000000000000000 ) ) ;
#17938 = DIRECTION ( 'NONE',  ( 0.000000000000000000, -0.7071067811865389130, -0.7071067811865561215 ) ) ;
#17939 = ORIENTED_EDGE ( 'NONE', *, *, #4357, .T. ) ;
#17940 = DIRECTION ( 'NONE',  ( 0.000000000000000000, 0.000000000000000000, 1.000000000000000000 ) ) ;
#17941 = ORIENTED_EDGE ( 'NONE', *, *, #16689, .T. ) ;
#17942 = ADVANCED_FACE ( 'NONE', ( #17684 ), #15969, .T. ) ;
#17943 = DIRECTION ( 'NONE',  ( 0.000000000000000000, 0.000000000000000000, 1.000000000000000000 ) ) ;
#17944 = CARTESIAN_POINT ( 'NONE',  ( 13.90576474687263264, 10.00000000000000000, -42.79754323328189969 ) ) ;
#17945 = CARTESIAN_POINT ( 'NONE',  ( 0.000000000000000000, 0.000000000000000000, 0.000000000000000000 ) ) ;
#17946 = ORIENTED_EDGE ( 'NONE', *, *, #50, .F. ) ;
#17947 = ORIENTED_EDGE ( 'NONE', *, *, #18062, .F. ) ;
#17948 = DIRECTION ( 'NONE',  ( -1.000000000000000000, -0.000000000000000000, 0.000000000000000000 ) ) ;
#17949 = DIRECTION ( 'NONE',  ( 6.123233995736766036E-17, -1.000000000000000000, 0.000000000000000000 ) ) ;
#17950 = CARTESIAN_POINT ( 'NONE',  ( 0.000000000000000000, 0.000000000000000000, 0.000000000000000000 ) ) ;
#17951 = ORIENTED_EDGE ( 'NONE', *, *, #8812, .F. ) ;
#17952 = AXIS2_PLACEMENT_3D ( 'NONE', #1948, #13679, #2054 ) ;
#17953 = LINE ( 'NONE', #6052, #13851 ) ;
#17954 = CARTESIAN_POINT ( 'NONE',  ( -90.00000000009001155, -10.00000000000001599, -5.000000000000005329 ) ) ;
#17955 = DIRECTION ( 'NONE',  ( 0.000000000000000000, -0.5877852522924801315, 0.8090169943749421222 ) ) ;
#17956 = VERTEX_POINT ( 'NONE', #5698 ) ;
#17957 = CARTESIAN_POINT ( 'NONE',  ( -5.686050877451574337, -5.768780236673276995, -1.000000000000000000 ) ) ;
#17958 = ORIENTED_EDGE ( 'NONE', *, *, #15623, .T. ) ;
#17959 = UNCERTAINTY_MEASURE_WITH_UNIT (LENGTH_MEASURE( 1.000000000000000082E-05 ), #11562, 'distance_accuracy_value', 'NONE');
#17960 = CARTESIAN_POINT ( 'NONE',  ( 10.00000000000000000, -1.335003989221234200, -56.23315539212691760 ) ) ;
#17961 = ORIENTED_EDGE ( 'NONE', *, *, #1845, .F. ) ;
#17962 = EDGE_CURVE ( 'NONE', #5480, #1893, #258, .T. ) ;
#17963 = EDGE_CURVE ( 'NONE', #9323, #15432, #4027, .T. ) ;
#17964 = AXIS2_PLACEMENT_3D ( 'NONE', #5551, #2406, #8221 ) ;
#17965 = ADVANCED_FACE ( 'NONE', ( #8730 ), #16164, .T. ) ;
#17966 = DIRECTION ( 'NONE',  ( -0.000000000000000000, 1.000000000000000000, -0.000000000000000000 ) ) ;
#17967 = FACE_OUTER_BOUND ( 'NONE', #665, .T. ) ;
#17968 = ORIENTED_EDGE ( 'NONE', *, *, #17263, .F. ) ;
#17969 = EDGE_LOOP ( 'NONE', ( #4946, #7443, #2871, #54 ) ) ;
#17970 = CARTESIAN_POINT ( 'NONE',  ( 0.000000000000000000, -2.357898499370431722, 2.818925648462311528E-15 ) ) ;
#17971 = EDGE_CURVE ( 'NONE', #5879, #5044, #16196, .T. ) ;
#17972 = ORIENTED_EDGE ( 'NONE', *, *, #15442, .F. ) ;
#17973 = CARTESIAN_POINT ( 'NONE',  ( 45.00000000000000000, 10.00000000000000000, 2.649999999999487432 ) ) ;
#17974 = ADVANCED_FACE ( 'NONE', ( #14728 ), #12868, .T. ) ;
#17975 = MECHANICAL_DESIGN_GEOMETRIC_PRESENTATION_REPRESENTATION (  '', ( #2773 ), #16763 ) ;
#17976 = ADVANCED_FACE ( 'NONE', ( #11511 ), #166, .F. ) ;
#17977 = CARTESIAN_POINT ( 'NONE',  ( -4.000000000000003553, 2.309401076758496263, -3.504269196027868905 ) ) ;
#17978 = VERTEX_POINT ( 'NONE', #17593 ) ;
#17979 = EDGE_LOOP ( 'NONE', ( #13456, #12833, #6064, #13080 ) ) ;
#17980 = CARTESIAN_POINT ( 'NONE',  ( -11.25000000000000355, 29.90000000000000213, 0.000000000000000000 ) ) ;
#17981 = DIRECTION ( 'NONE',  ( 0.000000000000000000, -1.000000000000000000, 0.000000000000000000 ) ) ;
#17982 = FACE_OUTER_BOUND ( 'NONE', #4716, .T. ) ;
#17983 = EDGE_LOOP ( 'NONE', ( #2888, #13849, #13087, #4639 ) ) ;
#17984 = DIRECTION ( 'NONE',  ( 0.000000000000000000, 0.000000000000000000, 1.000000000000000000 ) ) ;
#17985 = EDGE_CURVE ( 'NONE', #7161, #16102, #1504, .T. ) ;
#17986 = CARTESIAN_POINT ( 'NONE',  ( 0.000000000000000000, 0.5192545390863916310, 0.000000000000000000 ) ) ;
#17987 = CYLINDRICAL_SURFACE ( 'NONE', #7676, 0.7500000000000000000 ) ;
#17988 = CARTESIAN_POINT ( 'NONE',  ( 0.000000000000000000, 25.42247726998014912, 12.18267823974760411 ) ) ;
#17989 = ORIENTED_EDGE ( 'NONE', *, *, #669, .T. ) ;
#17990 = VECTOR ( 'NONE', #18421, 1000.000000000000000 ) ;
#17991 = DIRECTION ( 'NONE',  ( -1.000000000000000000, 0.000000000000000000, 0.000000000000000000 ) ) ;
#17992 = EDGE_LOOP ( 'NONE', ( #2553, #7483 ) ) ;
#17993 = CARTESIAN_POINT ( 'NONE',  ( 10.00000000000000000, 44.70888270294211253, -34.13306034420136825 ) ) ;
#17994 = CARTESIAN_POINT ( 'NONE',  ( 8.060728450267873768, -24.77235419320996357, 0.000000000000000000 ) ) ;
#17995 = ADVANCED_FACE ( 'NONE', ( #10076 ), #1678, .T. ) ;
#17996 = AXIS2_PLACEMENT_3D ( 'NONE', #16294, #3251, #17917 ) ;
#17997 = ORIENTED_EDGE ( 'NONE', *, *, #744, .F. ) ;
#17998 = ORIENTED_EDGE ( 'NONE', *, *, #10056, .F. ) ;
#17999 = CARTESIAN_POINT ( 'NONE',  ( 4.211405965630455661, 2.460463115436283932, -3.751298928144577882 ) ) ;
#18000 = LINE ( 'NONE', #13723, #8431 ) ;
#18001 = CYLINDRICAL_SURFACE ( 'NONE', #6282, 30.00000000000000711 ) ;
#18002 = AXIS2_PLACEMENT_3D ( 'NONE', #10004, #15820, #8845 ) ;
#18003 = CARTESIAN_POINT ( 'NONE',  ( -3.309651814758565180, -5.455921364805393026, -1.000000000000000000 ) ) ;
#18004 = CARTESIAN_POINT ( 'NONE',  ( -26.29305231718568336, -26.50000000000000000, -21.75302069950551953 ) ) ;
#18005 = ORIENTED_EDGE ( 'NONE', *, *, #4122, .T. ) ;
#18006 = FACE_OUTER_BOUND ( 'NONE', #1737, .T. ) ;
#18007 =( NAMED_UNIT ( * ) PLANE_ANGLE_UNIT ( ) SI_UNIT ( $, .RADIAN. ) );
#18008 = CARTESIAN_POINT ( 'NONE',  ( 10.00000000000000000, -27.94286728106395756, 3.730438010304225394 ) ) ;
#18009 = VERTEX_POINT ( 'NONE', #18735 ) ;
#18010 = EDGE_CURVE ( 'NONE', #2422, #6, #18346, .T. ) ;
#18011 = AXIS2_PLACEMENT_3D ( 'NONE', #9988, #15807, #4806 ) ;
#18012 = ORIENTED_EDGE ( 'NONE', *, *, #11983, .F. ) ;
#18013 = AXIS2_PLACEMENT_3D ( 'NONE', #13890, #4181, #8464 ) ;
#18014 = VERTEX_POINT ( 'NONE', #17328 ) ;
#18015 = AXIS2_PLACEMENT_3D ( 'NONE', #9167, #17937, #7645 ) ;
#18016 = ORIENTED_EDGE ( 'NONE', *, *, #6057, .F. ) ;
#18017 = DIRECTION ( 'NONE',  ( 0.000000000000000000, 0.000000000000000000, 1.000000000000000000 ) ) ;
#18018 = DIRECTION ( 'NONE',  ( 1.000000000000000000, 0.000000000000000000, 0.000000000000000000 ) ) ;
#18019 = DIRECTION ( 'NONE',  ( 0.000000000000000000, -0.8090169943749531134, 0.5877852522924653655 ) ) ;
#18020 = CARTESIAN_POINT ( 'NONE',  ( 0.000000000000000000, 27.94286728106393269, 3.730438010304423013 ) ) ;
#18021 = CARTESIAN_POINT ( 'NONE',  ( 5.000000000000000000, -61.03368945066446827, 15.61693798565473656 ) ) ;
#18022 = EDGE_CURVE ( 'NONE', #15880, #16509, #4652, .T. ) ;
#18023 = DIRECTION ( 'NONE',  ( 0.000000000000000000, 0.000000000000000000, 1.000000000000000000 ) ) ;
#18024 = DIRECTION ( 'NONE',  ( 0.000000000000000000, 0.5877852522924741363, -0.8090169943749466741 ) ) ;
#18025 = DIRECTION ( 'NONE',  ( 1.000000000000000000, 0.000000000000000000, 0.000000000000000000 ) ) ;
#18026 = ORIENTED_EDGE ( 'NONE', *, *, #13438, .T. ) ;
#18027 = DIRECTION ( 'NONE',  ( -0.000000000000000000, 0.000000000000000000, 1.000000000000000000 ) ) ;
#18028 = ORIENTED_EDGE ( 'NONE', *, *, #9457, .F. ) ;
#18029 = EDGE_CURVE ( 'NONE', #18365, #17515, #6475, .T. ) ;
#18030 = CARTESIAN_POINT ( 'NONE',  ( -56.50000000009000445, -34.99999999999999289, 3.817814120399276590E-13 ) ) ;
#18031 = LINE ( 'NONE', #4978, #15023 ) ;
#18032 = CIRCLE ( 'NONE', #8309, 2.041999999999999815 ) ;
#18033 = DIRECTION ( 'NONE',  ( -1.000000000000000000, -0.000000000000000000, -0.000000000000000000 ) ) ;
#18034 = EDGE_LOOP ( 'NONE', ( #13498, #9649 ) ) ;
#18035 = ORIENTED_EDGE ( 'NONE', *, *, #12921, .F. ) ;
#18036 = CLOSED_SHELL ( 'NONE', ( #12881, #11176, #17085, #14757, #12137, #6190, #4857, #8594, #8325, #5757, #11574, #5625, #17325, #12509, #2753, #11925, #14604, #18680, #14964, #9495, #10862, #6847, #13084, #7659, #1206, #16251, #5501 ) ) ;
#18037 = DIRECTION ( 'NONE',  ( 0.000000000000000000, 0.000000000000000000, 1.000000000000000000 ) ) ;
#18038 = CARTESIAN_POINT ( 'NONE',  ( -90.00000000009003998, 1.821459649775647449E-14, -5.746271514173173500E-15 ) ) ;
#18039 = DIRECTION ( 'NONE',  ( -1.000000000000000000, -0.000000000000000000, -0.000000000000000000 ) ) ;
#18040 = VERTEX_POINT ( 'NONE', #5793 ) ;
#18041 = PRODUCT_DEFINITION_SHAPE ( 'NONE', 'NONE',  #18841 ) ;
#18042 = AXIS2_PLACEMENT_3D ( 'NONE', #16324, #9083, #10608 ) ;
#18043 = DIRECTION ( 'NONE',  ( 0.000000000000000000, 0.000000000000000000, 1.000000000000000000 ) ) ;
#18044 = FACE_OUTER_BOUND ( 'NONE', #12525, .T. ) ;
#18045 = LINE ( 'NONE', #17676, #16354 ) ;
#18046 = ORIENTED_EDGE ( 'NONE', *, *, #1897, .F. ) ;
#18047 = CARTESIAN_POINT ( 'NONE',  ( 4.000000000000000888, 1.539600717838996990, -3.300726591567079815 ) ) ;
#18048 = ORIENTED_EDGE ( 'NONE', *, *, #3166, .F. ) ;
#18049 = CARTESIAN_POINT ( 'NONE',  ( 5.000000000000000000, -5.940243314904445349, 32.46095361140691438 ) ) ;
#18050 = ORIENTED_EDGE ( 'NONE', *, *, #13834, .T. ) ;
#18051 = DIRECTION ( 'NONE',  ( -1.000000000000000000, -0.000000000000000000, 0.000000000000000000 ) ) ;
#18052 = DIRECTION ( 'NONE',  ( -1.000000000000000000, -0.000000000000000000, -0.000000000000000000 ) ) ;
#18053 = EDGE_LOOP ( 'NONE', ( #9674, #12919, #234, #5539 ) ) ;
#18054 = ORIENTED_EDGE ( 'NONE', *, *, #9341, .F. ) ;
#18055 = CARTESIAN_POINT ( 'NONE',  ( -5.560781378645575757, 6.809993116116508640E-16, -4.000000000000000000 ) ) ;
#18056 =( LENGTH_UNIT ( ) NAMED_UNIT ( * ) SI_UNIT ( .MILLI., .METRE. ) );
#18057 = CIRCLE ( 'NONE', #14414, 24.00000000002399858 ) ;
#18058 = ORIENTED_EDGE ( 'NONE', *, *, #14289, .T. ) ;
#18059 = LINE ( 'NONE', #839, #18238 ) ;
#18060 = EDGE_CURVE ( 'NONE', #9749, #16034, #1009, .T. ) ;
#18061 = CARTESIAN_POINT ( 'NONE',  ( 0.000000000000000000, -17.25000000000000355, 27.50000000000000000 ) ) ;
#18062 = EDGE_CURVE ( 'NONE', #5529, #3221, #2923, .T. ) ;
#18063 = DIRECTION ( 'NONE',  ( 0.000000000000000000, -0.7071067811865535679, 0.7071067811865414665 ) ) ;
#18064 = VERTEX_POINT ( 'NONE', #13126 ) ;
#18065 = COLOUR_RGB ( '',1.000000000000000000, 0.9490196078431372140, 0.9098039215686274384 ) ;
#18066 = ADVANCED_FACE ( 'NONE', ( #4997 ), #3491, .T. ) ;
#18067 = ORIENTED_EDGE ( 'NONE', *, *, #15521, .F. ) ;
#18068 = CARTESIAN_POINT ( 'NONE',  ( -5.384454397937118664, 6.594054843588581554E-16, -4.484454397937119197 ) ) ;
#18069 = DIRECTION ( 'NONE',  ( 0.000000000000000000, 1.000000000000000000, 0.000000000000000000 ) ) ;
#18070 = DIRECTION ( 'NONE',  ( 1.000000000000000000, 0.000000000000000000, 0.000000000000000000 ) ) ;
#18071 = ORIENTED_EDGE ( 'NONE', *, *, #8562, .T. ) ;
#18072 = CARTESIAN_POINT ( 'NONE',  ( 129.9999999999999432, -30.00000000000000000, -125.0000000000000000 ) ) ;
#18073 = ADVANCED_FACE ( 'NONE', ( #4917 ), #15285, .F. ) ;
#18074 = DIRECTION ( 'NONE',  ( 0.000000000000000000, 0.000000000000000000, 1.000000000000000000 ) ) ;
#18075 = FACE_OUTER_BOUND ( 'NONE', #8544, .T. ) ;
#18076 = CARTESIAN_POINT ( 'NONE',  ( 4.197393957002303999, 7.772902908466098641E-14, -3.503767560748929810 ) ) ;
#18077 = VERTEX_POINT ( 'NONE', #18148 ) ;
#18078 = FACE_OUTER_BOUND ( 'NONE', #7051, .T. ) ;
#18080 = EDGE_CURVE ( 'NONE', #6022, #890, #11034, .T. ) ;
#18079 = ORIENTED_EDGE ( 'NONE', *, *, #305, .T. ) ;
#18081 = CARTESIAN_POINT ( 'NONE',  ( -4.154094228333820915, -2.398367420967594921, -3.721909803043257803 ) ) ;
#18082 = CYLINDRICAL_SURFACE ( 'NONE', #3752, 24.00000000002399858 ) ;
#18083 = STYLED_ITEM ( 'NONE', ( #12536 ), #4884 ) ;
#18084 = CIRCLE ( 'NONE', #9878, 2.649999999999992806 ) ;
#18085 = EDGE_CURVE ( 'NONE', #10072, #6237, #16832, .T. ) ;
#18086 = ADVANCED_FACE ( 'NONE', ( #17873 ), #3312, .T. ) ;
#18087 = ORIENTED_EDGE ( 'NONE', *, *, #18132, .T. ) ;
#18088 = EDGE_CURVE ( 'NONE', #11686, #3186, #11651, .T. ) ;
#18089 = ORIENTED_EDGE ( 'NONE', *, *, #17907, .T. ) ;
#18090 = CARTESIAN_POINT ( 'NONE',  ( 10.00000000000000000, -56.37237871411032586, -1.017308535512989609 ) ) ;
#18091 = CARTESIAN_POINT ( 'NONE',  ( 4.000000000000000000, 0.8378280264232961239, -3.220590601395640018 ) ) ;
#18093 = ADVANCED_FACE ( 'NONE', ( #1869 ), #15212, .T. ) ;
#18092 = FACE_OUTER_BOUND ( 'NONE', #1961, .T. ) ;
#18094 = CARTESIAN_POINT ( 'NONE',  ( -90.00000000009001155, -30.00000000000000000, -1.301042606982605321E-15 ) ) ;
#18095 = AXIS2_PLACEMENT_3D ( 'NONE', #8331, #8136, #3755 ) ;
#18096 = CARTESIAN_POINT ( 'NONE',  ( 10.00000000000000000, 61.03368945066456064, -15.61693798565434399 ) ) ;
#18097 = CIRCLE ( 'NONE', #11091, 2.500000000000000444 ) ;
#18098 = DIRECTION ( 'NONE',  ( -1.000000000000000000, 0.000000000000000000, 0.000000000000000000 ) ) ;
#18099 = ORIENTED_EDGE ( 'NONE', *, *, #15790, .F. ) ;
#18100 = DIRECTION ( 'NONE',  ( -1.000000000000000000, 0.000000000000000000, -0.000000000000000000 ) ) ;
#18101 = VECTOR ( 'NONE', #8590, 999.9999999999998863 ) ;
#18102 = CARTESIAN_POINT ( 'NONE',  ( 10.00000000000000000, 16.45250512421934630, -53.92768374110874419 ) ) ;
#18103 = VERTEX_POINT ( 'NONE', #12157 ) ;
#18104 = ORIENTED_EDGE ( 'NONE', *, *, #10869, .T. ) ;
#18105 = VERTEX_POINT ( 'NONE', #6527 ) ;
#18106 = VECTOR ( 'NONE', #11593, 1000.000000000000000 ) ;
#18107 = AXIS2_PLACEMENT_3D ( 'NONE', #15927, #12594, #4039 ) ;
#18108 = EDGE_LOOP ( 'NONE', ( #7138, #13668, #5584, #12799 ) ) ;
#18109 = CARTESIAN_POINT ( 'NONE',  ( 2.500000000000000000, 1.178949249685213863, -2.042000000000001148 ) ) ;
#18110 = CARTESIAN_POINT ( 'NONE',  ( -0.3789929286210603765, -30.00000000000000000, 24.99712712213256793 ) ) ;
#18111 = DIRECTION ( 'NONE',  ( -1.000000000000000000, 0.000000000000000000, 0.000000000000000000 ) ) ;
#18112 = ADVANCED_FACE ( 'NONE', ( #3210 ), #7669, .T. ) ;
#18113 = CARTESIAN_POINT ( 'NONE',  ( 10.00000000000000000, -49.49802920186203892, -26.71881558261783951 ) ) ;
#18114 = DIRECTION ( 'NONE',  ( -1.000000000000000000, 0.000000000000000000, 0.000000000000000000 ) ) ;
#18115 = LINE ( 'NONE', #3370, #7818 ) ;
#18116 = CARTESIAN_POINT ( 'NONE',  ( 0.1481481481481481122, -4.797713218419819903, 0.000000000000000000 ) ) ;
#18117 = VECTOR ( 'NONE', #15779, 1000.000000000000000 ) ;
#18118 = DIRECTION ( 'NONE',  ( -1.000000000000000000, 0.000000000000000000, 0.000000000000000000 ) ) ;
#18119 = ORIENTED_EDGE ( 'NONE', *, *, #8913, .F. ) ;
#18120 = FACE_OUTER_BOUND ( 'NONE', #2681, .T. ) ;
#18121 = VECTOR ( 'NONE', #10141, 1000.000000000000000 ) ;
#18122 = VERTEX_POINT ( 'NONE', #4829 ) ;
#18123 = DIRECTION ( 'NONE',  ( 0.000000000000000000, 0.000000000000000000, 1.000000000000000000 ) ) ;
#18124 = PLANE ( 'NONE',  #11502 ) ;
#18125 = ORIENTED_EDGE ( 'NONE', *, *, #3646, .T. ) ;
#18126 = VERTEX_POINT ( 'NONE', #10630 ) ;
#18127 = VECTOR ( 'NONE', #1613, 1000.000000000000000 ) ;
#18128 = CARTESIAN_POINT ( 'NONE',  ( 5.200000000000002842, 3.306546357697854226E-16, 2.700000000000000622 ) ) ;
#18129 = DIRECTION ( 'NONE',  ( 6.123233995736766036E-17, -1.000000000000000000, 0.000000000000000000 ) ) ;
#18130 = DIRECTION ( 'NONE',  ( -1.000000000000000000, -0.000000000000000000, -0.000000000000000000 ) ) ;
#18131 = VERTEX_POINT ( 'NONE', #3399 ) ;
#18132 = EDGE_CURVE ( 'NONE', #17139, #4385, #99, .T. ) ;
#18133 = AXIS2_PLACEMENT_3D ( 'NONE', #3475, #10510, #10699 ) ;
#18134 = AXIS2_PLACEMENT_3D ( 'NONE', #17435, #4384, #2960 ) ;
#18135 = ADVANCED_FACE ( 'NONE', ( #17967 ), #15018, .T. ) ;
#18136 = AXIS2_PLACEMENT_3D ( 'NONE', #2694, #1075, #14316 ) ;
#18137 = DIRECTION ( 'NONE',  ( 0.000000000000000000, 0.5877852522924684742, 0.8090169943749506709 ) ) ;
#18138 = FACE_BOUND ( 'NONE', #6590, .T. ) ;
#18139 = VECTOR ( 'NONE', #5926, 1000.000000000000000 ) ;
#18140 = DIRECTION ( 'NONE',  ( -1.000000000000000000, 0.000000000000000000, 0.000000000000000000 ) ) ;
#18141 = EDGE_LOOP ( 'NONE', ( #2792, #11109, #1036, #10743 ) ) ;
#18142 = CARTESIAN_POINT ( 'NONE',  ( -90.00000000009001155, -34.99999999999999289, 5.000000000000003553 ) ) ;
#18143 = ORIENTED_EDGE ( 'NONE', *, *, #1898, .T. ) ;
#18144 = CARTESIAN_POINT ( 'NONE',  ( 0.000000000000000000, 0.000000000000000000, 0.000000000000000000 ) ) ;
#18145 = VERTEX_POINT ( 'NONE', #9287 ) ;
#18146 =( REPRESENTATION_RELATIONSHIP ('NONE','NONE', #11014, #16765 ) REPRESENTATION_RELATIONSHIP_WITH_TRANSFORMATION ( #15449 )SHAPE_REPRESENTATION_RELATIONSHIP( ) );
#18147 = CARTESIAN_POINT ( 'NONE',  ( 10.00000000000000000, 16.60877409751168443, 20.32630374611190405 ) ) ;
#18148 = CARTESIAN_POINT ( 'NONE',  ( 21.00000000000000355, 2.789133085058097101E-16, -2.055000000000000160 ) ) ;
#18149 = AXIS2_PLACEMENT_3D ( 'NONE', #9426, #2188, #7994 ) ;
#18150 = ORIENTED_EDGE ( 'NONE', *, *, #12502, .F. ) ;
#18151 = ORIENTED_EDGE ( 'NONE', *, *, #14374, .T. ) ;
#18152 = CIRCLE ( 'NONE', #12681, 24.00000000002400569 ) ;
#18153 = FACE_OUTER_BOUND ( 'NONE', #576, .T. ) ;
#18154 = ORIENTED_EDGE ( 'NONE', *, *, #4305, .T. ) ;
#18155 = DIRECTION ( 'NONE',  ( 0.000000000000000000, 0.000000000000000000, 1.000000000000000000 ) ) ;
#18156 = CONICAL_SURFACE ( 'NONE', #529, 2.055000000000000160, 0.7853981633974639331 ) ;
#18157 = AXIS2_PLACEMENT_3D ( 'NONE', #5141, #9521, #8099 ) ;
#18158 = EDGE_CURVE ( 'NONE', #16191, #1279, #12251, .T. ) ;
#18159 = EDGE_CURVE ( 'NONE', #11786, #4356, #15579, .T. ) ;
#18160 = CARTESIAN_POINT ( 'NONE',  ( 0.000000000000000000, 0.000000000000000000, 0.000000000000000000 ) ) ;
#18161 = CIRCLE ( 'NONE', #13624, 2.649999999999999467 ) ;
#18162 = DIRECTION ( 'NONE',  ( -0.000000000000000000, 1.000000000000000000, -0.000000000000000000 ) ) ;
#18163 = ORIENTED_EDGE ( 'NONE', *, *, #2289, .T. ) ;
#18164 = CIRCLE ( 'NONE', #9040, 33.00000000003299760 ) ;
#18165 = CIRCLE ( 'NONE', #14526, 2.649999999999999467 ) ;
#18166 = ORIENTED_EDGE ( 'NONE', *, *, #12369, .T. ) ;
#18167 = DIRECTION ( 'NONE',  ( -1.000000000000000000, 1.224646799147352714E-16, 0.000000000000000000 ) ) ;
#18168 = VECTOR ( 'NONE', #12261, 1000.000000000000000 ) ;
#18169 = DIRECTION ( 'NONE',  ( -1.000000000000000000, 0.000000000000000000, 0.000000000000000000 ) ) ;
#18170 = DIRECTION ( 'NONE',  ( 0.000000000000000000, 0.000000000000000000, 1.000000000000000000 ) ) ;
#18171 = EDGE_LOOP ( 'NONE', ( #9598, #10961, #15998, #8311 ) ) ;
#18172 = DIRECTION ( 'NONE',  ( -1.000000000000000000, -0.000000000000000000, -0.000000000000000000 ) ) ;
#18173 = DIRECTION ( 'NONE',  ( -1.000000000000000000, 0.000000000000000000, -0.000000000000000000 ) ) ;
#18174 = CARTESIAN_POINT ( 'NONE',  ( -56.50000000009000445, -30.00000000000000000, -2.649999999999604228 ) ) ;
#18175 = EDGE_LOOP ( 'NONE', ( #5177, #4296, #18079, #15501 ) ) ;
#18176 = ORIENTED_EDGE ( 'NONE', *, *, #8664, .F. ) ;
#18177 = EDGE_CURVE ( 'NONE', #17129, #1734, #1921, .T. ) ;
#18178 = FACE_OUTER_BOUND ( 'NONE', #17029, .T. ) ;
#18179 = ADVANCED_FACE ( 'NONE', ( #12622 ), #12530, .T. ) ;
#18180 = ORIENTED_EDGE ( 'NONE', *, *, #13644, .T. ) ;
#18181 = CYLINDRICAL_SURFACE ( 'NONE', #15170, 2.649999999999999467 ) ;
#18182 = CARTESIAN_POINT ( 'NONE',  ( 10.00000000000000000, -5.117658387065794099E-13, -47.64999999999999858 ) ) ;
#18183 = AXIS2_PLACEMENT_3D ( 'NONE', #18800, #14228, #4232 ) ;
#18184 = PRODUCT_DEFINITION ( 'UNKNOWN', '', #18408, #7303 ) ;
#18185 = AXIS2_PLACEMENT_3D ( 'NONE', #3367, #13554, #16224 ) ;
#18186 = AXIS2_PLACEMENT_3D ( 'NONE', #5168, #9642, #9541 ) ;
#18187 = ORIENTED_EDGE ( 'NONE', *, *, #12014, .T. ) ;
#18188 = VECTOR ( 'NONE', #9478, 1000.000000000000000 ) ;
#18189 = VERTEX_POINT ( 'NONE', #6909 ) ;
#18190 = CARTESIAN_POINT ( 'NONE',  ( 10.00000000000000178, 0.000000000000000000, 0.000000000000000000 ) ) ;
#18191 = DIRECTION ( 'NONE',  ( 0.9914448613738104932, -0.1305261922200517399, 0.000000000000000000 ) ) ;
#18192 = FACE_OUTER_BOUND ( 'NONE', #13896, .T. ) ;
#18193 = CARTESIAN_POINT ( 'NONE',  ( 10.00000000000000000, 26.71881558261799228, -49.49802920186195365 ) ) ;
#18194 = AXIS2_PLACEMENT_3D ( 'NONE', #5336, #8005, #11144 ) ;
#18195 = CARTESIAN_POINT ( 'NONE',  ( 0.000000000000000000, 0.000000000000000000, 0.000000000000000000 ) ) ;
#18196 = VECTOR ( 'NONE', #11447, 999.9999999999997726 ) ;
#18197 = DIRECTION ( 'NONE',  ( 0.000000000000000000, 0.000000000000000000, 1.000000000000000000 ) ) ;
#18198 = EDGE_LOOP ( 'NONE', ( #17972, #1582, #15254, #1049 ) ) ;
#18199 = DIRECTION ( 'NONE',  ( -1.000000000000000000, -0.000000000000000000, 0.000000000000000000 ) ) ;
#18200 = EDGE_CURVE ( 'NONE', #9128, #16979, #17141, .T. ) ;
#18201 = EDGE_CURVE ( 'NONE', #1691, #6509, #14687, .T. ) ;
#18202 = EDGE_CURVE ( 'NONE', #5083, #6509, #15918, .T. ) ;
#18203 = CARTESIAN_POINT ( 'NONE',  ( 10.04305231718579705, -26.50000000000000000, 33.55933677959249195 ) ) ;
#18204 = EDGE_LOOP ( 'NONE', ( #6154, #12924, #13647, #18463 ) ) ;
#18205 = EDGE_CURVE ( 'NONE', #6567, #3837, #706, .T. ) ;
#18206 = ORIENTED_EDGE ( 'NONE', *, *, #14693, .T. ) ;
#18207 = AXIS2_PLACEMENT_3D ( 'NONE', #3838, #9648, #12596 ) ;
#18208 = VECTOR ( 'NONE', #2487, 1000.000000000000114 ) ;
#18209 = VERTEX_POINT ( 'NONE', #6632 ) ;
#18210 = VECTOR ( 'NONE', #4097, 1000.000000000000000 ) ;
#18211 = CIRCLE ( 'NONE', #7252, 5.000000000000004441 ) ;
#18212 = ORIENTED_EDGE ( 'NONE', *, *, #7521, .T. ) ;
#18213 = EDGE_CURVE ( 'NONE', #4773, #13137, #12441, .T. ) ;
#18214 = DIRECTION ( 'NONE',  ( 1.000000000000000000, 0.000000000000000000, 0.000000000000000000 ) ) ;
#18215 = DIRECTION ( 'NONE',  ( -0.000000000000000000, 1.000000000000000000, -0.000000000000000000 ) ) ;
#18216 =( NAMED_UNIT ( * ) SI_UNIT ( $, .STERADIAN. ) SOLID_ANGLE_UNIT ( ) );
#18217 = DIRECTION ( 'NONE',  ( -0.1586811557617541502, 1.606889522083424400E-16, -0.9873298794253692057 ) ) ;
#18218 = DIRECTION ( 'NONE',  ( 1.000000000000000000, -0.000000000000000000, -0.000000000000000000 ) ) ;
#18219 = PLANE ( 'NONE',  #15448 ) ;
#18220 = CIRCLE ( 'NONE', #10015, 8.099999999999999645 ) ;
#18221 = DIRECTION ( 'NONE',  ( -1.000000000000000000, -0.000000000000000000, -0.000000000000000000 ) ) ;
#18222 = CARTESIAN_POINT ( 'NONE',  ( 0.000000000000000000, 0.000000000000000000, 0.000000000000000000 ) ) ;
#18223 = ORIENTED_EDGE ( 'NONE', *, *, #13439, .F. ) ;
#18224 = CARTESIAN_POINT ( 'NONE',  ( 10.00000000000000000, 53.22058882792246237, -33.71303790549217183 ) ) ;
#18225 = VERTEX_POINT ( 'NONE', #15294 ) ;
#18226 = EDGE_CURVE ( 'NONE', #18412, #17183, #3138, .T. ) ;
#18227 = AXIS2_PLACEMENT_3D ( 'NONE', #7675, #17598, #6159 ) ;
#18228 = CYLINDRICAL_SURFACE ( 'NONE', #6185, 56.24900000005625600 ) ;
#18229 = DIRECTION ( 'NONE',  ( 1.000000000000000000, 0.000000000000000000, 0.000000000000000000 ) ) ;
#18230 = ORIENTED_EDGE ( 'NONE', *, *, #10124, .T. ) ;
#18231 = ORIENTED_EDGE ( 'NONE', *, *, #14715, .F. ) ;
#18232 = CARTESIAN_POINT ( 'NONE',  ( 4.078421086530217288, -3.990950201428958621, 0.000000000000000000 ) ) ;
#18233 = CARTESIAN_POINT ( 'NONE',  ( -26.29305231718611324, -39.99999999999999289, 19.10302069950493475 ) ) ;
#18234 = CARTESIAN_POINT ( 'NONE',  ( -1.747541505913277282, 3.837784562140256650, -3.503702292528906526 ) ) ;
#18235 = ORIENTED_EDGE ( 'NONE', *, *, #2143, .T. ) ;
#18236 = EDGE_CURVE ( 'NONE', #18040, #3486, #13780, .T. ) ;
#18237 = CIRCLE ( 'NONE', #15503, 56.24900000005625600 ) ;
#18238 = VECTOR ( 'NONE', #17879, 1000.000000000000114 ) ;
#18239 = DIRECTION ( 'NONE',  ( -1.000000000000000000, 0.000000000000000000, -0.000000000000000000 ) ) ;
#18240 = CARTESIAN_POINT ( 'NONE',  ( -6.259644161404860030E-16, -4.618802153517027165, -5.000000000000000000 ) ) ;
#18241 = CARTESIAN_POINT ( 'NONE',  ( 2.500000000000000000, 0.000000000000000000, 0.000000000000000000 ) ) ;
#18242 = ORIENTED_EDGE ( 'NONE', *, *, #11796, .F. ) ;
#18243 = FACE_OUTER_BOUND ( 'NONE', #14952, .T. ) ;
#18244 = ORIENTED_EDGE ( 'NONE', *, *, #10154, .F. ) ;
#18245 = CARTESIAN_POINT ( 'NONE',  ( 10.00000000000000000, -18.64666490672335186, -53.06836994729252410 ) ) ;
#18246 = VERTEX_POINT ( 'NONE', #5196 ) ;
#18247 = CARTESIAN_POINT ( 'NONE',  ( 0.000000000000000000, 10.00000000000000000, 0.000000000000000000 ) ) ;
#18248 = DIRECTION ( 'NONE',  ( -1.000000000000000000, 0.000000000000000000, 0.000000000000000000 ) ) ;
#18249 = CARTESIAN_POINT ( 'NONE',  ( -90.72413394419160682, 1.778525910263251795E-14, 4.947285117213269245 ) ) ;
#18250 = VERTEX_POINT ( 'NONE', #1111 ) ;
#18251 = EDGE_LOOP ( 'NONE', ( #15605, #6492, #9200, #9249, #6532 ) ) ;
#18252 = DIRECTION ( 'NONE',  ( -1.000000000000000000, 0.000000000000000000, 0.000000000000000000 ) ) ;
#18253 = AXIS2_PLACEMENT_3D ( 'NONE', #533, #4815, #7859 ) ;
#18254 =( LENGTH_UNIT ( ) NAMED_UNIT ( * ) SI_UNIT ( .MILLI., .METRE. ) );
#18255 = ORIENTED_EDGE ( 'NONE', *, *, #14388, .T. ) ;
#18256 = DIRECTION ( 'NONE',  ( 0.000000000000000000, 0.000000000000000000, 1.000000000000000000 ) ) ;
#18257 = ADVANCED_FACE ( 'NONE', ( #12724 ), #8049, .T. ) ;
#18258 = FACE_OUTER_BOUND ( 'NONE', #15236, .T. ) ;
#18259 = CYLINDRICAL_SURFACE ( 'NONE', #1442, 2.100000000000000089 ) ;
#18260 = ORIENTED_EDGE ( 'NONE', *, *, #9715, .T. ) ;
#18262 = VECTOR ( 'NONE', #17559, 999.9999999999998863 ) ;
#18261 = CYLINDRICAL_SURFACE ( 'NONE', #8835, 12.00000000001200284 ) ;
#18263 = EDGE_LOOP ( 'NONE', ( #6937, #16215, #10311, #6203 ) ) ;
#18264 = FACE_OUTER_BOUND ( 'NONE', #3572, .T. ) ;
#18265 = DIRECTION ( 'NONE',  ( 0.000000000000000000, 1.000000000000000000, 0.000000000000000000 ) ) ;
#18266 = EDGE_CURVE ( 'NONE', #3895, #205, #9484, .T. ) ;
#18267 = ORIENTED_EDGE ( 'NONE', *, *, #8524, .T. ) ;
#18268 = DIRECTION ( 'NONE',  ( 0.000000000000000000, 8.881784197001252323E-16, 1.000000000000000000 ) ) ;
#18269 = VERTEX_POINT ( 'NONE', #10910 ) ;
#18270 = LINE ( 'NONE', #5216, #12114 ) ;
#18271 = DIRECTION ( 'NONE',  ( -1.000000000000000000, 0.000000000000000000, -0.000000000000000000 ) ) ;
#18272 = ORIENTED_EDGE ( 'NONE', *, *, #18411, .T. ) ;
#18273 = EDGE_LOOP ( 'NONE', ( #492, #16894, #5147, #1229 ) ) ;
#18274 = SURFACE_STYLE_USAGE ( .BOTH. , #12469 ) ;
#18275 = EDGE_CURVE ( 'NONE', #6911, #2085, #12882, .T. ) ;
#18276 = EDGE_LOOP ( 'NONE', ( #7821, #5968, #7883, #15485 ) ) ;
#18277 = DIRECTION ( 'NONE',  ( 0.000000000000000000, 0.000000000000000000, 1.000000000000000000 ) ) ;
#18278 = CARTESIAN_POINT ( 'NONE',  ( 10.00000000000000000, 0.000000000000000000, 0.000000000000000000 ) ) ;
#18279 = VECTOR ( 'NONE', #9971, 1000.000000000000000 ) ;
#18280 = EDGE_LOOP ( 'NONE', ( #2266, #14594, #9278, #17536 ) ) ;
#18281 = EDGE_LOOP ( 'NONE', ( #16402, #4918, #10811, #5581 ) ) ;
#18282 = DIRECTION ( 'NONE',  ( 0.000000000000000000, 0.000000000000000000, 1.000000000000000000 ) ) ;
#18283 = CARTESIAN_POINT ( 'NONE',  ( 0.3865131578947368918, -23.49682122285426189, -2.000000000000000000 ) ) ;
#18284 = CARTESIAN_POINT ( 'NONE',  ( 5.000000000000000000, -29.03656532225574338, 15.68049343255986017 ) ) ;
#18285 = DIRECTION ( 'NONE',  ( 0.000000000000000000, 0.000000000000000000, 1.000000000000000000 ) ) ;
#18286 = VECTOR ( 'NONE', #16530, 1000.000000000000000 ) ;
#18287 = LINE ( 'NONE', #18580, #3911 ) ;
#18288 = DIRECTION ( 'NONE',  ( 0.9938152567191714803, 0.000000000000000000, -0.1110460963393456596 ) ) ;
#18289 = DIRECTION ( 'NONE',  ( 0.000000000000000000, -1.000000000000000000, 0.000000000000000000 ) ) ;
#18290 = ORIENTED_EDGE ( 'NONE', *, *, #12557, .F. ) ;
#18291 = CARTESIAN_POINT ( 'NONE',  ( -3.453038570459499024, -2.625189405340453419, -3.535263753545272891 ) ) ;
#18292 = CARTESIAN_POINT ( 'NONE',  ( -4.000000000000000000, -1.560351142792950618, -0.2242961665059814425 ) ) ;
#18293 = LINE ( 'NONE', #15540, #7995 ) ;
#18294 = CONTEXT_DEPENDENT_SHAPE_REPRESENTATION ( #635, #7223 ) ;
#18295 = EDGE_LOOP ( 'NONE', ( #2848, #15967, #4914, #5957 ) ) ;
#18296 = ORIENTED_EDGE ( 'NONE', *, *, #18656, .F. ) ;
#18297 = EDGE_CURVE ( 'NONE', #17607, #14062, #3686, .T. ) ;
#18298 = EDGE_CURVE ( 'NONE', #7917, #179, #14394, .T. ) ;
#18299 = ORIENTED_EDGE ( 'NONE', *, *, #4927, .F. ) ;
#18301 = LINE ( 'NONE', #789, #18441 ) ;
#18300 = AXIS2_PLACEMENT_3D ( 'NONE', #4038, #6501, #16707 ) ;
#18302 = EDGE_CURVE ( 'NONE', #18755, #12710, #927, .T. ) ;
#18303 = DIRECTION ( 'NONE',  ( -1.000000000000000000, -0.000000000000000000, 0.000000000000000000 ) ) ;
#18304 = CARTESIAN_POINT ( 'NONE',  ( -2.500000000000000888, 0.000000000000000000, -4.974599999999998801 ) ) ;
#18305 = CARTESIAN_POINT ( 'NONE',  ( -87.43997332177200121, 1.691927380938166737E-14, 6.475821446449876007 ) ) ;
#18306 = CARTESIAN_POINT ( 'NONE',  ( -79.64793068852898728, -34.99999999999999289, -34.51039329588756033 ) ) ;
#18307 = EDGE_CURVE ( 'NONE', #11293, #8684, #9670, .T. ) ;
#18308 = DIRECTION ( 'NONE',  ( -2.031314180040284764E-16, -1.000000000000000000, -1.301042606982601377E-16 ) ) ;
#18309 = CARTESIAN_POINT ( 'NONE',  ( -12.69999999999999929, 3.429011037612589670E-15, 28.00000000000000355 ) ) ;
#18310 = CARTESIAN_POINT ( 'NONE',  ( 0.000000000000000000, 3.000000000000000000, 0.000000000000000000 ) ) ;
#18311 = ORIENTED_EDGE ( 'NONE', *, *, #1681, .F. ) ;
#18312 = CARTESIAN_POINT ( 'NONE',  ( -87.43997332177200121, 1.691927380938166737E-14, 6.475821446449876007 ) ) ;
#18313 = VERTEX_POINT ( 'NONE', #5935 ) ;
#18314 = CARTESIAN_POINT ( 'NONE',  ( 10.00000000000000000, 50.69000562871642046, 24.68609584167177218 ) ) ;
#18315 = DIRECTION ( 'NONE',  ( 0.000000000000000000, 0.000000000000000000, -1.000000000000000000 ) ) ;
#18316 = ORIENTED_EDGE ( 'NONE', *, *, #14370, .F. ) ;
#18317 = EDGE_LOOP ( 'NONE', ( #16814, #8725, #11727, #15117 ) ) ;
#18318 = DIRECTION ( 'NONE',  ( -1.000000000000000000, 0.000000000000000000, 0.000000000000000000 ) ) ;
#18319 =( NAMED_UNIT ( * ) PLANE_ANGLE_UNIT ( ) SI_UNIT ( $, .RADIAN. ) );
#18320 = VECTOR ( 'NONE', #14197, 1000.000000000000000 ) ;
#18321 = DIRECTION ( 'NONE',  ( -1.000000000000000000, 0.000000000000000000, 0.000000000000000000 ) ) ;
#18322 = VERTEX_POINT ( 'NONE', #11379 ) ;
#18323 = ADVANCED_FACE ( 'NONE', ( #2902 ), #14424, .T. ) ;
#18324 = B_SPLINE_CURVE_WITH_KNOTS ( 'NONE', 3,
 ( #6625, #16815, #16905, #18047, #922 ),
 .UNSPECIFIED., .F., .F.,
 ( 4, 1, 4 ),
 ( 0.000000000000000000, 0.002309401076758505790, 0.004618802153517011580 ),
 .UNSPECIFIED. ) ;
#18325 = EDGE_CURVE ( 'NONE', #3589, #18400, #6173, .T. ) ;
#18326 = CYLINDRICAL_SURFACE ( 'NONE', #5344, 24.00000000002399858 ) ;
#18327 = EDGE_CURVE ( 'NONE', #10887, #14354, #4372, .T. ) ;
#18328 = DIRECTION ( 'NONE',  ( -0.000000000000000000, 1.000000000000000000, -0.000000000000000000 ) ) ;
#18329 = CYLINDRICAL_SURFACE ( 'NONE', #12404, 2.649999999999999467 ) ;
#18330 = FACE_OUTER_BOUND ( 'NONE', #8103, .T. ) ;
#18331 = AXIS2_PLACEMENT_3D ( 'NONE', #16937, #14700, #51 ) ;
#18332 = ORIENTED_EDGE ( 'NONE', *, *, #17728, .F. ) ;
#18333 = UNCERTAINTY_MEASURE_WITH_UNIT (LENGTH_MEASURE( 1.000000000000000082E-05 ), #17749, 'distance_accuracy_value', 'NONE');
#18334 = VECTOR ( 'NONE', #16974, 1000.000000000000000 ) ;
#18335 = DIRECTION ( 'NONE',  ( -1.000000000000000000, -0.000000000000000000, -0.000000000000000000 ) ) ;
#18336 = ORIENTED_EDGE ( 'NONE', *, *, #11072, .T. ) ;
#18337 = EDGE_CURVE ( 'NONE', #2698, #3664, #14517, .T. ) ;
#18338 = CARTESIAN_POINT ( 'NONE',  ( 0.000000000000000000, 0.000000000000000000, 0.000000000000000000 ) ) ;
#18339 = CARTESIAN_POINT ( 'NONE',  ( 5.000000000000000000, -41.62350880771954564, 47.29147401531940886 ) ) ;
#18340 = CYLINDRICAL_SURFACE ( 'NONE', #13999, 25.00000000000000000 ) ;
#18341 = VERTEX_POINT ( 'NONE', #16047 ) ;
#18342 = ORIENTED_EDGE ( 'NONE', *, *, #2199, .T. ) ;
#18343 = DIRECTION ( 'NONE',  ( -1.000000000000000000, 0.000000000000000000, 0.000000000000000000 ) ) ;
#18344 = ORIENTED_EDGE ( 'NONE', *, *, #8931, .T. ) ;
#18345 = CARTESIAN_POINT ( 'NONE',  ( 0.000000000000000000, 0.000000000000000000, 0.000000000000000000 ) ) ;
#18346 = CIRCLE ( 'NONE', #9202, 20.00000000000000000 ) ;
#18347 = VECTOR ( 'NONE', #9420, 1000.000000000000000 ) ;
#18348 = CARTESIAN_POINT ( 'NONE',  ( 12.49999999999999289, 0.000000000000000000, 0.000000000000000000 ) ) ;
#18349 = DIRECTION ( 'NONE',  ( 0.000000000000000000, 0.000000000000000000, 1.000000000000000000 ) ) ;
#18350 = VERTEX_POINT ( 'NONE', #16144 ) ;
#18351 = DIRECTION ( 'NONE',  ( 0.000000000000000000, 0.000000000000000000, 1.000000000000000000 ) ) ;
#18352 = ORIENTED_EDGE ( 'NONE', *, *, #3262, .T. ) ;
#18353 = DIRECTION ( 'NONE',  ( 0.000000000000000000, 0.000000000000000000, -1.000000000000000000 ) ) ;
#18354 = DIRECTION ( 'NONE',  ( 0.000000000000000000, 0.8090169943749445647, 0.5877852522924770229 ) ) ;
#18355 = CARTESIAN_POINT ( 'NONE',  ( 11.14999999999999680, 3.073863465859856794E-15, -25.10000000000000142 ) ) ;
#18356 = ORIENTED_EDGE ( 'NONE', *, *, #2597, .F. ) ;
#18357 = DIRECTION ( 'NONE',  ( -0.000000000000000000, 1.287488025362403787E-15, 1.000000000000000000 ) ) ;
#18358 = EDGE_CURVE ( 'NONE', #4317, #657, #11676, .T. ) ;
#18359 = ORIENTED_EDGE ( 'NONE', *, *, #10174, .T. ) ;
#18360 = AXIS2_PLACEMENT_3D ( 'NONE', #13565, #16234, #15089 ) ;
#18361 = DIRECTION ( 'NONE',  ( -1.000000000000000000, 0.000000000000000000, 0.000000000000000000 ) ) ;
#18362 = DIRECTION ( 'NONE',  ( -1.000000000000000000, -0.000000000000000000, -0.000000000000000000 ) ) ;
#18363 = VERTEX_POINT ( 'NONE', #58 ) ;
#18364 = VERTEX_POINT ( 'NONE', #13189 ) ;
#18365 = VERTEX_POINT ( 'NONE', #5579 ) ;
#18366 = CARTESIAN_POINT ( 'NONE',  ( 10.00000000000000000, -18.64666490672335186, -53.06836994729252410 ) ) ;
#18367 = DIRECTION ( 'NONE',  ( 0.000000000000000000, -1.000000000000000000, 0.000000000000000000 ) ) ;
#18368 = EDGE_CURVE ( 'NONE', #2985, #18678, #3097, .T. ) ;
#18369 = ORIENTED_EDGE ( 'NONE', *, *, #5486, .F. ) ;
#18370 = EDGE_CURVE ( 'NONE', #16606, #1536, #11048, .T. ) ;
#18371 = VERTEX_POINT ( 'NONE', #14617 ) ;
#18372 = CARTESIAN_POINT ( 'NONE',  ( 10.00000000000000000, 26.45033635316149301, 36.40576474687247099 ) ) ;
#18373 = CARTESIAN_POINT ( 'NONE',  ( 4.000000000000000888, 0.8228435280416209752, -3.430609588141487976 ) ) ;
#18374 = CYLINDRICAL_SURFACE ( 'NONE', #6284, 24.00000000002399858 ) ;
#18375 = DIRECTION ( 'NONE',  ( 1.000000000000000000, 0.000000000000000000, 0.000000000000000000 ) ) ;
#18376 = DIRECTION ( 'NONE',  ( 0.000000000000000000, 0.000000000000000000, 1.000000000000000000 ) ) ;
#18377 = CARTESIAN_POINT ( 'NONE',  ( 0.000000000000000000, -14.19907017806852245, -22.07705612348854984 ) ) ;
#18378 = CARTESIAN_POINT ( 'NONE',  ( 3.367778697655221307E-15, -17.25000000000000355, -27.50000000000000000 ) ) ;
#18379 = VERTEX_POINT ( 'NONE', #1651 ) ;
#18380 = CARTESIAN_POINT ( 'NONE',  ( 0.000000000000000000, -1.335003989221234200, -56.23315539212691760 ) ) ;
#18381 = DIRECTION ( 'NONE',  ( 0.000000000000000000, 1.000000000000000000, 0.000000000000000000 ) ) ;
#18382 = DIRECTION ( 'NONE',  ( -1.000000000000000000, 0.000000000000000000, 0.000000000000000000 ) ) ;
#18383 = DIRECTION ( 'NONE',  ( -0.000000000000000000, 1.000000000000000000, -0.000000000000000000 ) ) ;
#18384 = ORIENTED_EDGE ( 'NONE', *, *, #5629, .T. ) ;
#18385 = ORIENTED_EDGE ( 'NONE', *, *, #2348, .F. ) ;
#18386 = ORIENTED_EDGE ( 'NONE', *, *, #10693, .F. ) ;
#18387 = AXIS2_PLACEMENT_3D ( 'NONE', #6228, #9179, #3190 ) ;
#18388 = CARTESIAN_POINT ( 'NONE',  ( 10.00000000000000000, -12.18267823974732522, -25.42247726998028057 ) ) ;
#18389 = CARTESIAN_POINT ( 'NONE',  ( 5.000000000000000000, 5.940243314904213534, 32.46095361140695701 ) ) ;
#18390 = AXIS2_PLACEMENT_3D ( 'NONE', #3979, #4071, #5296 ) ;
#18391 = LINE ( 'NONE', #12589, #7865 ) ;
#18392 = AXIS2_PLACEMENT_3D ( 'NONE', #3133, #10367, #1797 ) ;
#18393 = CARTESIAN_POINT ( 'NONE',  ( 10.00000000000000000, 0.000000000000000000, 0.000000000000000000 ) ) ;
#18394 = DIRECTION ( 'NONE',  ( -1.000000000000000000, 0.000000000000000000, -0.000000000000000000 ) ) ;
#18395 = CARTESIAN_POINT ( 'NONE',  ( 0.000000000000000000, 0.000000000000000000, 0.000000000000000000 ) ) ;
#18396 = CARTESIAN_POINT ( 'NONE',  ( 0.000000000000000000, 0.000000000000000000, 0.000000000000000000 ) ) ;
#18397 = CARTESIAN_POINT ( 'NONE',  ( -26.29305231718584324, -26.50000000000000000, 21.75302069950530637 ) ) ;
#18398 = ORIENTED_EDGE ( 'NONE', *, *, #7857, .F. ) ;
#18399 = CARTESIAN_POINT ( 'NONE',  ( 10.00000000000000000, 46.27827401617404490, 31.97297851452441364 ) ) ;
#18400 = VERTEX_POINT ( 'NONE', #143 ) ;
#18401 = CARTESIAN_POINT ( 'NONE',  ( 0.000000000000000000, 0.000000000000000000, -25.03750572909317285 ) ) ;
#18402 = CARTESIAN_POINT ( 'NONE',  ( -117.1020693116508085, -30.00000000000000000, 22.34080595179777262 ) ) ;
#18403 = VERTEX_POINT ( 'NONE', #5850 ) ;
#18404 = ORIENTED_EDGE ( 'NONE', *, *, #1151, .T. ) ;
#18405 = EDGE_CURVE ( 'NONE', #38, #1366, #11760, .T. ) ;
#18406 = CARTESIAN_POINT ( 'NONE',  ( -3.098410542199071749, -7.060458129626440815, -1.000000000000000000 ) ) ;
#18407 = APPLICATION_PROTOCOL_DEFINITION ( 'draft international standard', 'automotive_design', 1998, #8284 ) ;
#18408 = PRODUCT_DEFINITION_FORMATION_WITH_SPECIFIED_SOURCE ( 'ANY', '', #11327, .NOT_KNOWN. ) ;
#18409 = AXIS2_PLACEMENT_3D ( 'NONE', #6712, #16612, #715 ) ;
#18411 = EDGE_CURVE ( 'NONE', #5435, #5558, #10737, .T. ) ;
#18410 = DIRECTION ( 'NONE',  ( -1.000000000000000000, -0.000000000000000000, -0.000000000000000000 ) ) ;
#18412 = VERTEX_POINT ( 'NONE', #18623 ) ;
#18413 = AXIS2_PLACEMENT_3D ( 'NONE', #12346, #14066, #7971 ) ;
#18414 = VECTOR ( 'NONE', #17324, 1000.000000000000000 ) ;
#18415 = EDGE_CURVE ( 'NONE', #11571, #13362, #14698, .T. ) ;
#18416 = CARTESIAN_POINT ( 'NONE',  ( 0.000000000000000000, 0.000000000000000000, 0.000000000000000000 ) ) ;
#18417 = DIRECTION ( 'NONE',  ( -1.000000000000000000, 0.000000000000000000, -0.000000000000000000 ) ) ;
#18418 = VECTOR ( 'NONE', #13411, 1000.000000000000000 ) ;
#18419 = COLOUR_RGB ( '',1.000000000000000000, 0.9490196078431372140, 0.9098039215686274384 ) ;
#18420 = CARTESIAN_POINT ( 'NONE',  ( 2.500000000000000000, 2.357898499370432166, -2.385244779468109755E-15 ) ) ;
#18421 = DIRECTION ( 'NONE',  ( -1.000000000000000000, 0.000000000000000000, 0.000000000000000000 ) ) ;
#18422 = EDGE_CURVE ( 'NONE', #104, #13512, #2812, .T. ) ;
#18423 = CIRCLE ( 'NONE', #1412, 24.00000000002399858 ) ;
#18424 = CARTESIAN_POINT ( 'NONE',  ( 10.00000000000000000, 0.000000000000000000, 0.000000000000000000 ) ) ;
#18425 = VECTOR ( 'NONE', #16208, 1000.000000000000000 ) ;
#18426 = ORIENTED_EDGE ( 'NONE', *, *, #5862, .T. ) ;
#18427 = CARTESIAN_POINT ( 'NONE',  ( -117.1020693116508085, -38.00000000000000000, 22.34080595179777262 ) ) ;
#18428 = DIRECTION ( 'NONE',  ( -1.000000000000000000, 0.000000000000000000, 0.000000000000000000 ) ) ;
#18429 = FACE_OUTER_BOUND ( 'NONE', #6627, .T. ) ;
#18430 = ORIENTED_EDGE ( 'NONE', *, *, #4590, .F. ) ;
#18431 = ORIENTED_EDGE ( 'NONE', *, *, #16822, .T. ) ;
#18432 = EDGE_CURVE ( 'NONE', #11956, #11483, #14338, .T. ) ;
#18433 = CARTESIAN_POINT ( 'NONE',  ( 0.000000000000000000, -55.51919907100644735, -9.823366686501268319 ) ) ;
#18434 = EDGE_CURVE ( 'NONE', #15870, #17590, #2536, .T. ) ;
#18435 = ORIENTED_EDGE ( 'NONE', *, *, #15399, .F. ) ;
#18436 = DIRECTION ( 'NONE',  ( 0.000000000000000000, 0.000000000000000000, -1.000000000000000000 ) ) ;
#18437 = AXIS2_PLACEMENT_3D ( 'NONE', #7374, #4528, #10337 ) ;
#18438 = CIRCLE ( 'NONE', #7770, 24.00000000002399858 ) ;
#18439 = AXIS2_PLACEMENT_3D ( 'NONE', #4312, #3249, #4582 ) ;
#18440 = EDGE_CURVE ( 'NONE', #1108, #6670, #11485, .T. ) ;
#18441 = VECTOR ( 'NONE', #10768, 1000.000000000000000 ) ;
#18442 = CIRCLE ( 'NONE', #12046, 2.649999999999992806 ) ;
#18443 = EDGE_CURVE ( 'NONE', #15928, #2263, #17305, .T. ) ;
#18444 = LINE ( 'NONE', #842, #7756 ) ;
#18445 = DIRECTION ( 'NONE',  ( 0.000000000000000000, -0.7071067811865535679, 0.7071067811865414665 ) ) ;
#18446 = ORIENTED_EDGE ( 'NONE', *, *, #8262, .T. ) ;
#18447 = CARTESIAN_POINT ( 'NONE',  ( 0.000000000000000000, -34.99999999999999289, 20.00000000000000000 ) ) ;
#18448 = ADVANCED_FACE ( 'NONE', ( #7183 ), #13008, .T. ) ;
#18449 = AXIS2_PLACEMENT_3D ( 'NONE', #18476, #16671, #769 ) ;
#18450 = ORIENTED_EDGE ( 'NONE', *, *, #111, .F. ) ;
#18451 = DIRECTION ( 'NONE',  ( -0.000000000000000000, -1.000000000000000000, 0.000000000000000000 ) ) ;
#18452 = DIRECTION ( 'NONE',  ( 0.000000000000000000, 0.000000000000000000, 1.000000000000000000 ) ) ;
#18454 = CIRCLE ( 'NONE', #13883, 12.00000000001200462 ) ;
#18453 = CARTESIAN_POINT ( 'NONE',  ( -26.29305231718568336, -34.99999999999999289, -21.75302069950551953 ) ) ;
#18455 = ORIENTED_EDGE ( 'NONE', *, *, #9291, .F. ) ;
#18456 = LINE ( 'NONE', #5416, #18717 ) ;
#18457 = ORIENTED_EDGE ( 'NONE', *, *, #7563, .F. ) ;
#18458 = CIRCLE ( 'NONE', #18753, 63.00000000006298961 ) ;
#18459 = CARTESIAN_POINT ( 'NONE',  ( 10.00000000000000000, 49.49802920186260735, -26.71881558261677370 ) ) ;
#18460 = DIRECTION ( 'NONE',  ( 1.000000000000000000, 0.000000000000000000, 0.000000000000000000 ) ) ;
#18461 = AXIS2_PLACEMENT_3D ( 'NONE', #5206, #12741, #18445 ) ;
#18462 = ORIENTED_EDGE ( 'NONE', *, *, #6302, .F. ) ;
#18463 = ORIENTED_EDGE ( 'NONE', *, *, #3767, .T. ) ;
#18464 = CIRCLE ( 'NONE', #7195, 24.00000000002399858 ) ;
#18465 = DIRECTION ( 'NONE',  ( -1.000000000000000000, 0.000000000000000000, -0.000000000000000000 ) ) ;
#18466 =( NAMED_UNIT ( * ) PLANE_ANGLE_UNIT ( ) SI_UNIT ( $, .RADIAN. ) );
#18467 = ORIENTED_EDGE ( 'NONE', *, *, #15364, .T. ) ;
#18468 = CARTESIAN_POINT ( 'NONE',  ( 0.000000000000000000, -33.71303790549312396, 53.22058882792185841 ) ) ;
#18469 = LINE ( 'NONE', #16953, #9163 ) ;
#18470 = VECTOR ( 'NONE', #18394, 1000.000000000000000 ) ;
#18471 = ADVANCED_FACE ( 'NONE', ( #9264 ), #16604, .F. ) ;
#18472 = VECTOR ( 'NONE', #8816, 1000.000000000000000 ) ;
#18473 = AXIS2_PLACEMENT_3D ( 'NONE', #5068, #12214, #18023 ) ;
#18474 = ORIENTED_EDGE ( 'NONE', *, *, #10546, .T. ) ;
#18475 = VERTEX_POINT ( 'NONE', #9364 ) ;
#18476 = CARTESIAN_POINT ( 'NONE',  ( 0.000000000000000000, -30.00000000000000000, 0.000000000000000000 ) ) ;
#18477 = FACE_OUTER_BOUND ( 'NONE', #11867, .T. ) ;
#18478 = CARTESIAN_POINT ( 'NONE',  ( -90.00000000009001155, -49.14213562373095812, 5.000000000000003553 ) ) ;
#18479 = CARTESIAN_POINT ( 'NONE',  ( 32.50000000000000000, -26.50000000000000000, 3.680389326632394941E-13 ) ) ;
#18480 = FACE_OUTER_BOUND ( 'NONE', #12512, .T. ) ;
#18481 = LINE ( 'NONE', #11245, #6147 ) ;
#18482 = AXIS2_PLACEMENT_3D ( 'NONE', #17489, #5788, #13207 ) ;
#18483 = DIRECTION ( 'NONE',  ( -1.000000000000000000, -0.000000000000000000, -0.000000000000000000 ) ) ;
#18484 = EDGE_LOOP ( 'NONE', ( #5791, #4342, #3698, #7740 ) ) ;
#18485 = DIRECTION ( 'NONE',  ( -0.000000000000000000, 1.000000000000000000, -0.000000000000000000 ) ) ;
#18486 = DIRECTION ( 'NONE',  ( -1.000000000000000000, -0.000000000000000000, -0.000000000000000000 ) ) ;
#18487 = CIRCLE ( 'NONE', #13929, 2.700000000000000622 ) ;
#18488 = CARTESIAN_POINT ( 'NONE',  ( 0.000000000000000000, 0.000000000000000000, 0.000000000000000000 ) ) ;
#18489 = CARTESIAN_POINT ( 'NONE',  ( 4.000000000000000000, 2.309401076758497151, -3.433295621305379353 ) ) ;
#18490 = CIRCLE ( 'NONE', #16976, 33.00000000003299760 ) ;
#18491 = ITEM_DEFINED_TRANSFORMATION ( 'NONE', 'NONE', #17502,  #8017 ) ;
#18492 = ORIENTED_EDGE ( 'NONE', *, *, #3183, .T. ) ;
#18493 = B_SPLINE_CURVE_WITH_KNOTS ( 'NONE', 3,
 ( #3666, #6511, #9462, #1002, #2423, #5369 ),
 .UNSPECIFIED., .F., .F.,
 ( 4, 2, 4 ),
 ( 0.002365888236228001588, 0.003551327329835089319, 0.004736766423442177049 ),
 .UNSPECIFIED. ) ;
#18494 = ADVANCED_FACE ( 'NONE', ( #12026 ), #17665, .T. ) ;
#18495 = ORIENTED_EDGE ( 'NONE', *, *, #7511, .F. ) ;
#18496 = VECTOR ( 'NONE', #14514, 1000.000000000000000 ) ;
#18497 = ORIENTED_EDGE ( 'NONE', *, *, #12961, .F. ) ;
#18498 = CIRCLE ( 'NONE', #5112, 24.00000000002399858 ) ;
#18499 = CYLINDRICAL_SURFACE ( 'NONE', #13581, 41.00000000000000000 ) ;
#18500 = AXIS2_PLACEMENT_3D ( 'NONE', #8698, #4248, #16039 ) ;
#18501 = CIRCLE ( 'NONE', #10292, 12.00000000001200462 ) ;
#18502 = DIRECTION ( 'NONE',  ( 0.000000000000000000, 0.000000000000000000, -1.000000000000000000 ) ) ;
#18503 = CARTESIAN_POINT ( 'NONE',  ( 10.00000000000000000, -1.335003989222025123, 56.23315539212689629 ) ) ;
#18504 = DIRECTION ( 'NONE',  ( 1.000000000000000000, -0.000000000000000000, -0.000000000000000000 ) ) ;
#18505 = DIRECTION ( 'NONE',  ( 1.000000000000000000, 0.000000000000000000, 0.000000000000000000 ) ) ;
#18506 = DIRECTION ( 'NONE',  ( 1.000000000000000000, 0.000000000000000000, 0.000000000000000000 ) ) ;
#18507 = CARTESIAN_POINT ( 'NONE',  ( 10.00000000000000000, -9.823366686501049827, 55.51919907100648999 ) ) ;
#18508 = ORIENTED_EDGE ( 'NONE', *, *, #6558, .T. ) ;
#18509 = CARTESIAN_POINT ( 'NONE',  ( 10.00000000000000000, 0.000000000000000000, 0.000000000000000000 ) ) ;
#18510 = ORIENTED_EDGE ( 'NONE', *, *, #8556, .T. ) ;
#18511 = EDGE_CURVE ( 'NONE', #11459, #9292, #4664, .T. ) ;
#18512 = DIRECTION ( 'NONE',  ( 0.000000000000000000, 0.000000000000000000, -1.000000000000000000 ) ) ;
#18513 = DIRECTION ( 'NONE',  ( 0.000000000000000000, 0.000000000000000000, 1.000000000000000000 ) ) ;
#18514 = AXIS2_PLACEMENT_3D ( 'NONE', #14990, #16141, #13279 ) ;
#18515 = EDGE_LOOP ( 'NONE', ( #4530, #15228, #11943, #13173 ) ) ;
#18516 = DIRECTION ( 'NONE',  ( 0.000000000000000000, -1.000000000000000000, 0.000000000000000000 ) ) ;
#18517 = DIRECTION ( 'NONE',  ( 1.000000000000000000, 6.123233995736766036E-17, -6.123233995736764803E-17 ) ) ;
#18518 = VECTOR ( 'NONE', #4108, 1000.000000000000000 ) ;
#18519 = ADVANCED_FACE ( 'NONE', ( #3471 ), #2040, .T. ) ;
#18520 = CARTESIAN_POINT ( 'NONE',  ( 0.000000000000000000, 0.000000000000000000, 0.000000000000000000 ) ) ;
#18521 = VERTEX_POINT ( 'NONE', #14994 ) ;
#18522 = AXIS2_PLACEMENT_3D ( 'NONE', #18782, #6980, #15836 ) ;
#18523 = AXIS2_PLACEMENT_3D ( 'NONE', #4744, #9030, #14851 ) ;
#18524 =( REPRESENTATION_RELATIONSHIP ('NONE','NONE', #11014, #2517 ) REPRESENTATION_RELATIONSHIP_WITH_TRANSFORMATION ( #2576 )SHAPE_REPRESENTATION_RELATIONSHIP( ) );
#18525 = DIRECTION ( 'NONE',  ( -0.08031988216184954288, 0.000000000000000000, -0.9967691390334607604 ) ) ;
#18526 = DIRECTION ( 'NONE',  ( 0.000000000000000000, 0.9876883405951383255, -0.1564344650402276493 ) ) ;
#18527 = AXIS2_PLACEMENT_3D ( 'NONE', #6198, #16120, #1825 ) ;
#18528 = DIRECTION ( 'NONE',  ( -1.000000000000000000, -0.000000000000000000, -0.000000000000000000 ) ) ;
#18529 = FACE_OUTER_BOUND ( 'NONE', #15292, .T. ) ;
#18530 = CIRCLE ( 'NONE', #15190, 30.00000000000000000 ) ;
#18531 = AXIS2_PLACEMENT_3D ( 'NONE', #10075, #18644, #11312 ) ;
#18532 = CARTESIAN_POINT ( 'NONE',  ( 10.00000000000000000, 0.000000000000000000, 0.000000000000000000 ) ) ;
#18533 = EDGE_LOOP ( 'NONE', ( #12748, #18087 ) ) ;
#18534 = LINE ( 'NONE', #7182, #18121 ) ;
#18535 = CARTESIAN_POINT ( 'NONE',  ( 10.00000000000000000, -39.14194549634336084, -40.58063702438384013 ) ) ;
#18536 = CARTESIAN_POINT ( 'NONE',  ( 10.00000000000000000, 0.000000000000000000, 0.000000000000000000 ) ) ;
#18537 = ORIENTED_EDGE ( 'NONE', *, *, #6083, .T. ) ;
#18538 = ORIENTED_EDGE ( 'NONE', *, *, #7794, .T. ) ;
#18539 = DIRECTION ( 'NONE',  ( -1.000000000000000000, 0.000000000000000000, 0.000000000000000000 ) ) ;
#18540 = ORIENTED_EDGE ( 'NONE', *, *, #17564, .T. ) ;
#18541 = DIRECTION ( 'NONE',  ( -1.000000000000000000, -0.000000000000000000, 0.000000000000000000 ) ) ;
#18542 = AXIS2_PLACEMENT_3D ( 'NONE', #16275, #16382, #13059 ) ;
#18543 = EDGE_CURVE ( 'NONE', #11085, #4094, #13183, .T. ) ;
#18544 = CIRCLE ( 'NONE', #13083, 12.00000000001200640 ) ;
#18545 = CARTESIAN_POINT ( 'NONE',  ( 0.000000000000000000, -30.00000000000000000, -41.00000000000000000 ) ) ;
#18546 = CARTESIAN_POINT ( 'NONE',  ( -90.38553543446691663, 1.000000000000018208, -4.784491867360616268 ) ) ;
#18547 = ADVANCED_FACE ( 'NONE', ( #13476 ), #13385, .T. ) ;
#18548 = ORIENTED_EDGE ( 'NONE', *, *, #5762, .T. ) ;
#18549 = EDGE_CURVE ( 'NONE', #17226, #3517, #17147, .T. ) ;
#18550 = EDGE_CURVE ( 'NONE', #7064, #16165, #5587, .T. ) ;
#18551 = CIRCLE ( 'NONE', #2120, 2.649999999999999467 ) ;
#18552 = VERTEX_POINT ( 'NONE', #611 ) ;
#18553 = DIRECTION ( 'NONE',  ( 1.000000000000000000, 0.000000000000000000, 0.000000000000000000 ) ) ;
#18554 = CARTESIAN_POINT ( 'NONE',  ( 4.999999999999999112, -61.47135697633788709, 13.79392154159114092 ) ) ;
#18555 = CARTESIAN_POINT ( 'NONE',  ( 10.00000000000000000, 27.94286728106393269, 3.730438010304423013 ) ) ;
#18556 = ORIENTED_EDGE ( 'NONE', *, *, #3579, .F. ) ;
#18557 = DIRECTION ( 'NONE',  ( 1.000000000000000000, 0.000000000000000000, 0.000000000000000000 ) ) ;
#18558 = ORIENTED_EDGE ( 'NONE', *, *, #11905, .T. ) ;
#18559 = VECTOR ( 'NONE', #8337, 1000.000000000000000 ) ;
#18560 = EDGE_CURVE ( 'NONE', #15930, #11128, #10781, .T. ) ;
#18561 = FACE_OUTER_BOUND ( 'NONE', #1065, .T. ) ;
#18562 = CARTESIAN_POINT ( 'NONE',  ( 0.000000000000000000, 0.000000000000000000, -2.000000000000000000 ) ) ;
#18563 = ORIENTED_EDGE ( 'NONE', *, *, #18236, .T. ) ;
#18564 = EDGE_LOOP ( 'NONE', ( #7601, #18796, #2814, #14088 ) ) ;
#18565 = DIRECTION ( 'NONE',  ( 1.000000000000000000, 0.000000000000000000, 0.000000000000000000 ) ) ;
#18566 = EDGE_CURVE ( 'NONE', #13852, #475, #15616, .T. ) ;
#18567 = ORIENTED_EDGE ( 'NONE', *, *, #11905, .F. ) ;
#18568 = DIRECTION ( 'NONE',  ( -1.000000000000000000, 0.000000000000000000, -0.000000000000000000 ) ) ;
#18569 = DIRECTION ( 'NONE',  ( -1.000000000000000000, -0.000000000000000000, 0.000000000000000000 ) ) ;
#18570 = EDGE_CURVE ( 'NONE', #10824, #2993, #9229, .T. ) ;
#18571 = VECTOR ( 'NONE', #15944, 1000.000000000000000 ) ;
#18572 = ORIENTED_EDGE ( 'NONE', *, *, #17120, .F. ) ;
#18573 = EDGE_CURVE ( 'NONE', #17109, #17226, #1938, .T. ) ;
#18574 = ORIENTED_EDGE ( 'NONE', *, *, #725, .F. ) ;
#18575 = DIRECTION ( 'NONE',  ( 0.000000000000000000, -0.9876883405951359940, -0.1564344650402419989 ) ) ;
#18576 = CARTESIAN_POINT ( 'NONE',  ( -10.00000000000000000, 0.000000000000000000, 0.000000000000000000 ) ) ;
#18577 = CARTESIAN_POINT ( 'NONE',  ( 10.00000000000000000, -33.95787273855277988, 45.00825343885009033 ) ) ;
#18578 = FACE_BOUND ( 'NONE', #14889, .T. ) ;
#18579 =( BOUNDED_SURFACE ( )  B_SPLINE_SURFACE ( 3, 2, ( 
 ( #945, #6826, #16650 ),
 ( #16936, #13704, #5210 ),
 ( #9301, #2257, #5011 ),
 ( #3889, #6739, #10820 ),
 ( #3609, #9691, #8270 ),
 ( #16840, #14071, #1031 ) ),
 .UNSPECIFIED., .F., .F., .F. ) 
 B_SPLINE_SURFACE_WITH_KNOTS ( ( 4, 2, 4 ),
 ( 3, 3 ),
 ( 0.02032853247518126225, 0.02278863295364821212, 0.02524873343211516200 ),
 ( 0.000000000000000000, 1.000000000000000000 ),
 .UNSPECIFIED. ) 
 GEOMETRIC_REPRESENTATION_ITEM ( )  RATIONAL_B_SPLINE_SURFACE ( (
 ( 1.000000000000000000, 0.8047781615896835161, 1.000000000000000000),
 ( 1.000000000000000000, 0.8123767586291043008, 1.000000000000000000),
 ( 1.000000000000000000, 0.8190662415562011134, 1.000000000000000000),
 ( 1.000000000000000000, 0.8192361015671398849, 1.000000000000000000),
 ( 1.000000000000000000, 0.8126135807102121689, 1.000000000000000000),
 ( 1.000000000000000000, 0.8047712338318585568, 1.000000000000000000) ) ) 
 REPRESENTATION_ITEM ( '' )  SURFACE ( )  );
#18580 = CARTESIAN_POINT ( 'NONE',  ( 2.500000000000000000, 2.357898499370431722, -2.818925648462311528E-15 ) ) ;
#18581 = LINE ( 'NONE', #1341, #18320 ) ;
#18582 = DIRECTION ( 'NONE',  ( 1.000000000000000000, -0.000000000000000000, -0.000000000000000000 ) ) ;
#18583 = ORIENTED_EDGE ( 'NONE', *, *, #14586, .T. ) ;
#18584 = DIRECTION ( 'NONE',  ( 0.000000000000000000, 0.000000000000000000, 1.000000000000000000 ) ) ;
#18585 = ADVANCED_FACE ( 'NONE', ( #10504 ), #12222, .T. ) ;
#18586 = CIRCLE ( 'NONE', #6723, 4.799999999999998934 ) ;
#18587 = CARTESIAN_POINT ( 'NONE',  ( 32.50000000000000000, -34.99999999999999289, 2.650000000000367617 ) ) ;
#18588 = CARTESIAN_POINT ( 'NONE',  ( 32.50000000000000000, -26.50000000000000000, -2.649999999999631317 ) ) ;
#18589 = DIRECTION ( 'NONE',  ( 0.000000000000000000, -0.3090169943749548898, 0.9510565162951511997 ) ) ;
#18590 = ORIENTED_EDGE ( 'NONE', *, *, #8831, .F. ) ;
#18591 = ORIENTED_EDGE ( 'NONE', *, *, #8429, .F. ) ;
#18592 = CARTESIAN_POINT ( 'NONE',  ( 12.49999999999999289, 27.00000000000000000, 0.000000000000000000 ) ) ;
#18593 = DIRECTION ( 'NONE',  ( -1.000000000000000000, 0.000000000000000000, 0.000000000000000000 ) ) ;
#18594 = ORIENTED_EDGE ( 'NONE', *, *, #14021, .T. ) ;
#18595 = PRESENTATION_STYLE_ASSIGNMENT (( #2587 ) ) ;
#18596 = DIRECTION ( 'NONE',  ( -1.000000000000000000, 0.000000000000000000, 0.000000000000000000 ) ) ;
#18597 = CARTESIAN_POINT ( 'NONE',  ( 2.500000000000000000, -2.357898499370432166, 3.035766082959412415E-15 ) ) ;
#18598 = CARTESIAN_POINT ( 'NONE',  ( 5.000000000000000000, 24.97244012287581327, -57.83923611457294101 ) ) ;
#18599 = DIRECTION ( 'NONE',  ( -1.000000000000000000, 0.000000000000000000, 0.000000000000000000 ) ) ;
#18600 = EDGE_LOOP ( 'NONE', ( #8297, #8935, #18651, #1224, #17939 ) ) ;
#18601 = DIRECTION ( 'NONE',  ( 0.000000000000000000, 0.000000000000000000, -1.000000000000000000 ) ) ;
#18602 = ORIENTED_EDGE ( 'NONE', *, *, #8885, .F. ) ;
#18603 = EDGE_CURVE ( 'NONE', #6825, #4781, #18031, .T. ) ;
#18604 = CARTESIAN_POINT ( 'NONE',  ( 10.00000000000000000, 0.000000000000000000, 0.000000000000000000 ) ) ;
#18605 = CARTESIAN_POINT ( 'NONE',  ( 13.90576474687299680, 10.00000000000000000, 40.14754323328178742 ) ) ;
#18606 = EDGE_LOOP ( 'NONE', ( #14666, #12247, #6430, #5193 ) ) ;
#18607 = FACE_OUTER_BOUND ( 'NONE', #18251, .T. ) ;
#18608 = AXIS2_PLACEMENT_3D ( 'NONE', #16277, #14050, #14137 ) ;
#18609 = DIRECTION ( 'NONE',  ( 0.1242487463281444493, 7.285838599102589797E-17, -0.9922511018063343569 ) ) ;
#18610 = CARTESIAN_POINT ( 'NONE',  ( -10.00000000000000000, 0.000000000000000000, 0.000000000000000000 ) ) ;
#18611 = ORIENTED_EDGE ( 'NONE', *, *, #12027, .T. ) ;
#18612 = CIRCLE ( 'NONE', #14351, 56.24900000005625600 ) ;
#18613 = ADVANCED_FACE ( 'NONE', ( #1847 ), #3378, .T. ) ;
#18614 = FACE_OUTER_BOUND ( 'NONE', #16568, .T. ) ;
#18615 = DIRECTION ( 'NONE',  ( 0.000000000000000000, 0.000000000000000000, 1.000000000000000000 ) ) ;
#18616 = LINE ( 'NONE', #15856, #4809 ) ;
#18617 = DIRECTION ( 'NONE',  ( -1.000000000000000000, -0.000000000000000000, -0.000000000000000000 ) ) ;
#18618 = EDGE_CURVE ( 'NONE', #202, #186, #8920, .T. ) ;
#18619 = DIRECTION ( 'NONE',  ( 0.000000000000000000, 0.000000000000000000, -1.000000000000000000 ) ) ;
#18620 = ORIENTED_EDGE ( 'NONE', *, *, #16222, .T. ) ;
#18621 = AXIS2_PLACEMENT_3D ( 'NONE', #14372, #9993, #10269 ) ;
#18622 = DIRECTION ( 'NONE',  ( 0.000000000000000000, 0.000000000000000000, 1.000000000000000000 ) ) ;
#18623 = CARTESIAN_POINT ( 'NONE',  ( -1.128893538851230005, 11.24999999999999467, 23.47286943213250154 ) ) ;
#18624 = CARTESIAN_POINT ( 'NONE',  ( 0.2499999999999966416, -8.096141056083448362, -1.000000000000000000 ) ) ;
#18625 = ORIENTED_EDGE ( 'NONE', *, *, #17159, .T. ) ;
#18626 = EDGE_LOOP ( 'NONE', ( #13338, #8672 ) ) ;
#18627 = APPLICATION_CONTEXT ( 'automotive_design' ) ;
#18628 = FACE_OUTER_BOUND ( 'NONE', #2005, .T. ) ;
#18629 = SURFACE_STYLE_FILL_AREA ( #13972 ) ;
#18630 = ORIENTED_EDGE ( 'NONE', *, *, #9592, .F. ) ;
#18631 = CARTESIAN_POINT ( 'NONE',  ( 10.00000000000000000, 26.20671763660628528, 1.489278925039608570 ) ) ;
#18632 = PRODUCT_DEFINITION_SHAPE ( 'NONE', 'NONE',  #8300 ) ;
#18633 = LINE ( 'NONE', #3019, #18106 ) ;
#18634 = AXIS2_PLACEMENT_3D ( 'NONE', #14899, #699, #605 ) ;
#18635 = FACE_OUTER_BOUND ( 'NONE', #1996, .T. ) ;
#18636 = ORIENTED_EDGE ( 'NONE', *, *, #6558, .F. ) ;
#18637 = DIRECTION ( 'NONE',  ( -0.000000000000000000, 1.000000000000000000, -0.000000000000000000 ) ) ;
#18638 = ORIENTED_EDGE ( 'NONE', *, *, #12990, .T. ) ;
#18639 = CARTESIAN_POINT ( 'NONE',  ( -1.317756351988340180, 3.857995168970202116, -0.04852650426601388955 ) ) ;
#18640 = CARTESIAN_POINT ( 'NONE',  ( 0.2500000000000002220, 0.000000000000000000, 0.000000000000000000 ) ) ;
#18641 = ORIENTED_EDGE ( 'NONE', *, *, #9468, .F. ) ;
#18642 = PLANE ( 'NONE',  #7814 ) ;
#18643 = ORIENTED_EDGE ( 'NONE', *, *, #15339, .F. ) ;
#18644 = DIRECTION ( 'NONE',  ( -1.000000000000000000, -0.000000000000000000, -0.000000000000000000 ) ) ;
#18645 = CARTESIAN_POINT ( 'NONE',  ( 13.90576474687263264, 10.00000000000000000, -42.79754323328189969 ) ) ;
#18646 = ORIENTED_EDGE ( 'NONE', *, *, #17547, .F. ) ;
#18647 = EDGE_LOOP ( 'NONE', ( #10040, #13863, #2870, #4508 ) ) ;
#18648 = DIRECTION ( 'NONE',  ( -1.000000000000000000, 0.000000000000000000, 0.000000000000000000 ) ) ;
#18649 = SHAPE_REPRESENTATION_RELATIONSHIP ( 'NONE' , 'NONE' ,  #18682, #9198 ) ;
#18650 = VECTOR ( 'NONE', #3868, 1000.000000000000000 ) ;
#18651 = ORIENTED_EDGE ( 'NONE', *, *, #9121, .F. ) ;
#18652 = CARTESIAN_POINT ( 'NONE',  ( 10.00000000000000000, 1.335003989222417697, -56.23315539212688918 ) ) ;
#18653 = CARTESIAN_POINT ( 'NONE',  ( 0.000000000000000000, 10.00000000000000000, -30.00000000000000000 ) ) ;
#18654 = AXIS2_PLACEMENT_3D ( 'NONE', #14392, #17711, #16104 ) ;
#18655 = ADVANCED_FACE ( 'NONE', ( #3843 ), #18228, .T. ) ;
#18656 = EDGE_CURVE ( 'NONE', #16471, #15168, #9843, .T. ) ;
#18657 = EDGE_CURVE ( 'NONE', #4975, #18105, #718, .T. ) ;
#18658 = DIRECTION ( 'NONE',  ( -1.000000000000000000, -0.000000000000000000, 0.000000000000000000 ) ) ;
#18659 = VERTEX_POINT ( 'NONE', #15651 ) ;
#18660 = ADVANCED_FACE ( 'NONE', ( #8233 ), #13835, .T. ) ;
#18661 = CIRCLE ( 'NONE', #10442, 24.00000000002399858 ) ;
#18662 = EDGE_LOOP ( 'NONE', ( #18697, #5734, #4808, #11683 ) ) ;
#18663 = DIRECTION ( 'NONE',  ( 0.000000000000000000, -0.8910065241883626808, -0.4539904997395568520 ) ) ;
#18664 = FACE_OUTER_BOUND ( 'NONE', #5577, .T. ) ;
#18665 = CARTESIAN_POINT ( 'NONE',  ( 5.000000000000000000, -24.97244012287543669, 57.83923611457311154 ) ) ;
#18666 = CARTESIAN_POINT ( 'NONE',  ( 21.00000000000000355, 0.000000000000000000, 0.000000000000000000 ) ) ;
#18667 = EDGE_CURVE ( 'NONE', #13789, #10958, #3761, .T. ) ;
#18668 = DIRECTION ( 'NONE',  ( 0.000000000000000000, 0.000000000000000000, 1.000000000000000000 ) ) ;
#18669 = CARTESIAN_POINT ( 'NONE',  ( -90.00000000009003998, 1.821459649775647449E-14, -5.746271514173173500E-15 ) ) ;
#18670 = CARTESIAN_POINT ( 'NONE',  ( 10.00000000000000000, -26.49895292617967257, -49.76630880786338196 ) ) ;
#18671 = ORIENTED_EDGE ( 'NONE', *, *, #3579, .T. ) ;
#18672 = CARTESIAN_POINT ( 'NONE',  ( -0.5449313310646672903, -4.304185902836978883, -3.316620875263469159 ) ) ;
#18673 = DIRECTION ( 'NONE',  ( 0.000000000000000000, 0.000000000000000000, 1.000000000000000000 ) ) ;
#18674 = LINE ( 'NONE', #11629, #9384 ) ;
#18675 = LINE ( 'NONE', #15338, #2524 ) ;
#18676 = EDGE_CURVE ( 'NONE', #11921, #11704, #2219, .T. ) ;
#18677 = EDGE_CURVE ( 'NONE', #11098, #16951, #18661, .T. ) ;
#18678 = VERTEX_POINT ( 'NONE', #8326 ) ;
#18679 = EDGE_CURVE ( 'NONE', #4919, #14211, #6507, .T. ) ;
#18680 = ADVANCED_FACE ( 'NONE', ( #16798 ), #804, .T. ) ;
#18681 = EDGE_LOOP ( 'NONE', ( #18296, #27, #18005, #123 ) ) ;
#18682 = SHAPE_REPRESENTATION ( 'base plate', ( #8017 ), #3161 ) ;
#18683 = LINE ( 'NONE', #7151, #12665 ) ;
#18684 = DIRECTION ( 'NONE',  ( -1.000000000000000000, -0.000000000000000000, 0.000000000000000000 ) ) ;
#18685 = ORIENTED_EDGE ( 'NONE', *, *, #13318, .F. ) ;
#18686 = LINE ( 'NONE', #5825, #12423 ) ;
#18687 = CARTESIAN_POINT ( 'NONE',  ( 10.00000000000000000, 1.017308535513159695, -56.37237871411032586 ) ) ;
#18688 = STYLED_ITEM ( 'NONE', ( #12731 ), #10770 ) ;
#18689 = DIRECTION ( 'NONE',  ( 0.000000000000000000, -0.8090169943749402348, -0.5877852522924830181 ) ) ;
#18690 = DIRECTION ( 'NONE',  ( 0.000000000000000000, 0.000000000000000000, -1.000000000000000000 ) ) ;
#18691 = CARTESIAN_POINT ( 'NONE',  ( -8.060728450267886203, -24.77235419320996002, 0.000000000000000000 ) ) ;
#18692 = VERTEX_POINT ( 'NONE', #7933 ) ;
#18693 = DIRECTION ( 'NONE',  ( 1.000000000000000000, 0.000000000000000000, 0.000000000000000000 ) ) ;
#18694 = ORIENTED_EDGE ( 'NONE', *, *, #4566, .T. ) ;
#18695 = FILL_AREA_STYLE_COLOUR ( '', #4969 ) ;
#18696 = CARTESIAN_POINT ( 'NONE',  ( -6.259644161404860030E-16, -4.618802153517027165, -3.433295621305388234 ) ) ;
#18697 = ORIENTED_EDGE ( 'NONE', *, *, #17493, .F. ) ;
#18698 = PRODUCT_CONTEXT ( 'NONE', #7187, 'mechanical' ) ;
#18699 = CARTESIAN_POINT ( 'NONE',  ( 0.000000000000000000, 0.000000000000000000, -0.2800830152838844622 ) ) ;
#18700 = VERTEX_POINT ( 'NONE', #14122 ) ;
#18701 = AXIS2_PLACEMENT_3D ( 'NONE', #16463, #14561, #10553 ) ;
#18702 = EDGE_CURVE ( 'NONE', #5078, #4891, #17743, .T. ) ;
#18703 = ORIENTED_EDGE ( 'NONE', *, *, #2432, .T. ) ;
#18704 = DIRECTION ( 'NONE',  ( 1.000000000000000000, 0.000000000000000000, 0.000000000000000000 ) ) ;
#18705 = FACE_OUTER_BOUND ( 'NONE', #2738, .T. ) ;
#18706 = DIRECTION ( 'NONE',  ( 0.000000000000000000, 0.000000000000000000, 1.000000000000000000 ) ) ;
#18707 = DIRECTION ( 'NONE',  ( -1.000000000000000000, 0.000000000000000000, 0.000000000000000000 ) ) ;
#18708 = CARTESIAN_POINT ( 'NONE',  ( -11.15000000000000391, 0.000000000000000000, 0.000000000000000000 ) ) ;
#18709 = ORIENTED_EDGE ( 'NONE', *, *, #2759, .T. ) ;
#18710 = PRODUCT_DEFINITION_FORMATION_WITH_SPECIFIED_SOURCE ( 'ANY', '', #4043, .NOT_KNOWN. ) ;
#18711 = CARTESIAN_POINT ( 'NONE',  ( -90.00000000009001155, -13.00000000000001776, -1.301042606982603940E-15 ) ) ;
#18712 = DIRECTION ( 'NONE',  ( 1.000000000000000000, 0.000000000000000000, 0.000000000000000000 ) ) ;
#18713 = CARTESIAN_POINT ( 'NONE',  ( 0.000000000000000000, 0.000000000000000000, 0.000000000000000000 ) ) ;
#18714 = ORIENTED_EDGE ( 'NONE', *, *, #6787, .T. ) ;
#18715 = VECTOR ( 'NONE', #12541, 1000.000000000000114 ) ;
#18716 = ORIENTED_EDGE ( 'NONE', *, *, #3545, .F. ) ;
#18717 = VECTOR ( 'NONE', #14168, 1000.000000000000000 ) ;
#18718 = DIRECTION ( 'NONE',  ( -1.000000000000000000, -0.000000000000000000, -0.000000000000000000 ) ) ;
#18719 = SURFACE_SIDE_STYLE ('',( #12917 ) ) ;
#18720 = ORIENTED_EDGE ( 'NONE', *, *, #13664, .T. ) ;
#18721 = ADVANCED_FACE ( 'NONE', ( #13750 ), #10883, .T. ) ;
#18722 = CIRCLE ( 'NONE', #8377, 56.24900000005624889 ) ;
#18723 = FACE_BOUND ( 'NONE', #5706, .T. ) ;
#18724 = AXIS2_PLACEMENT_3D ( 'NONE', #4167, #152, #11677 ) ;
#18726 = CIRCLE ( 'NONE', #176, 0.7500000000000000000 ) ;
#18725 = DIRECTION ( 'NONE',  ( 0.000000000000000000, 1.000000000000000000, 0.000000000000000000 ) ) ;
#18727 = EDGE_LOOP ( 'NONE', ( #8577, #3503, #15472, #3939 ) ) ;
#18728 = DIRECTION ( 'NONE',  ( 0.000000000000000000, 0.5877852522924741363, -0.8090169943749465631 ) ) ;
#18729 = VERTEX_POINT ( 'NONE', #16714 ) ;
#18730 = PLANE ( 'NONE',  #2975 ) ;
#18731 = ORIENTED_EDGE ( 'NONE', *, *, #16459, .F. ) ;
#18732 = CYLINDRICAL_SURFACE ( 'NONE', #5925, 2.500000000000000444 ) ;
#18733 = ORIENTED_EDGE ( 'NONE', *, *, #7130, .F. ) ;
#18734 = CARTESIAN_POINT ( 'NONE',  ( 10.00000000000000000, 50.69000562871642046, -24.68609584167177218 ) ) ;
#18735 = CARTESIAN_POINT ( 'NONE',  ( 0.000000000000000000, 31.97297851452492168, -46.27827401617368963 ) ) ;
#18736 = AXIS2_PLACEMENT_3D ( 'NONE', #14256, #2626, #9963 ) ;
#18737 = ORIENTED_EDGE ( 'NONE', *, *, #13528, .T. ) ;
#18738 = VERTEX_POINT ( 'NONE', #3662 ) ;
#18739 = VECTOR ( 'NONE', #17844, 1000.000000000000000 ) ;
#18740 = EDGE_CURVE ( 'NONE', #17177, #7394, #2419, .T. ) ;
#18741 = DIRECTION ( 'NONE',  ( 0.000000000000000000, 0.000000000000000000, 1.000000000000000000 ) ) ;
#18742 = CIRCLE ( 'NONE', #15393, 2.649999999999999467 ) ;
#18743 = EDGE_LOOP ( 'NONE', ( #8216, #12619, #8075, #13604 ) ) ;
#18744 = DIRECTION ( 'NONE',  ( 0.000000000000000000, 1.000000000000000000, 0.000000000000000000 ) ) ;
#18745 = AXIS2_PLACEMENT_3D ( 'NONE', #5186, #12322, #15479 ) ;
#18746 = AXIS2_PLACEMENT_3D ( 'NONE', #14423, #7091, #4335 ) ;
#18747 = CIRCLE ( 'NONE', #9914, 0.1000000000000028644 ) ;
#18748 = EDGE_CURVE ( 'NONE', #79, #3360, #2869, .T. ) ;
#18749 = DIRECTION ( 'NONE',  ( -0.000000000000000000, 0.000000000000000000, -1.000000000000000000 ) ) ;
#18750 = AXIS2_PLACEMENT_3D ( 'NONE', #6993, #11366, #17184 ) ;
#18751=STYLED_ITEM('',(#18883),#3693);
#18752 = ORIENTED_EDGE ( 'NONE', *, *, #8599, .F. ) ;
#18753 = AXIS2_PLACEMENT_3D ( 'NONE', #16963, #3919, #7046 ) ;
#18754 = CIRCLE ( 'NONE', #2327, 24.00000000002399503 ) ;
#18755 = VERTEX_POINT ( 'NONE', #8131 ) ;
#18756 = CARTESIAN_POINT ( 'NONE',  ( 0.000000000000000000, 0.000000000000000000, -55.00000000000000000 ) ) ;
#18757 = CIRCLE ( 'NONE', #1421, 24.00000000002399858 ) ;
#18758 = CARTESIAN_POINT ( 'NONE',  ( 2.500000000000000000, -1.178949249685214307, 2.042000000000001592 ) ) ;
#18759 = DIRECTION ( 'NONE',  ( -1.000000000000000000, 0.000000000000000000, 0.000000000000000000 ) ) ;
#18760 = CARTESIAN_POINT ( 'NONE',  ( -10.00000000000000000, 0.000000000000000000, 0.000000000000000000 ) ) ;
#18761 = EDGE_CURVE ( 'NONE', #11459, #18189, #18057, .T. ) ;
#18762 = DIRECTION ( 'NONE',  ( -1.000000000000000000, -0.000000000000000000, 0.000000000000000000 ) ) ;
#18763 = CARTESIAN_POINT ( 'NONE',  ( 10.00000000000000000, -22.76987570971544272, 23.88582760061473564 ) ) ;
#18764 = DIRECTION ( 'NONE',  ( -1.000000000000000000, -0.000000000000000000, 0.000000000000000000 ) ) ;
#18765 = ORIENTED_EDGE ( 'NONE', *, *, #18159, .F. ) ;
#18766 = CARTESIAN_POINT ( 'NONE',  ( 0.000000000000000000, 2.357898499370431722, -2.818925648462311528E-15 ) ) ;
#18767 = FACE_OUTER_BOUND ( 'NONE', #11566, .T. ) ;
#18768 = PRODUCT_DEFINITION ( 'UNKNOWN', '', #14449, #17041 ) ;
#18769 = EDGE_LOOP ( 'NONE', ( #16717, #9134, #3912, #8247 ) ) ;
#18770 = LINE ( 'NONE', #14391, #17303 ) ;
#18771 = LINE ( 'NONE', #6092, #6163 ) ;
#18772 = CIRCLE ( 'NONE', #10545, 24.00000000002399858 ) ;
#18773 = AXIS2_PLACEMENT_3D ( 'NONE', #10651, #10825, #15137 ) ;
#18774 = ORIENTED_EDGE ( 'NONE', *, *, #13401, .T. ) ;
#18775 = AXIS2_PLACEMENT_3D ( 'NONE', #8170, #12832, #15500 ) ;
#18776 = AXIS2_PLACEMENT_3D ( 'NONE', #13880, #18451, #5411 ) ;
#18777 = ORIENTED_EDGE ( 'NONE', *, *, #5972, .F. ) ;
#18778 = DIRECTION ( 'NONE',  ( -0.1586811557617541224, 1.606889522083433522E-16, -0.9873298794253690946 ) ) ;
#18779 = CYLINDRICAL_SURFACE ( 'NONE', #7922, 24.00000000002399503 ) ;
#18780 = AXIS2_PLACEMENT_3D ( 'NONE', #13328, #16265, #361 ) ;
#18781 = ORIENTED_EDGE ( 'NONE', *, *, #8759, .T. ) ;
#18782 = CARTESIAN_POINT ( 'NONE',  ( 10.00000000000000000, 18.38754094778241210, 53.29895248911682870 ) ) ;
#18783 = ADVANCED_FACE ( 'NONE', ( #5263 ), #12598, .F. ) ;
#18784 = DIRECTION ( 'NONE',  ( -1.000000000000000000, 0.000000000000000000, -0.000000000000000000 ) ) ;
#18785 = ADVANCED_FACE ( 'NONE', ( #2884 ), #17372, .T. ) ;
#18786 = AXIS2_PLACEMENT_3D ( 'NONE', #7739, #17751, #9265 ) ;
#18787 = ADVANCED_FACE ( 'NONE', ( #7264, #17456 ), #11363, .F. ) ;
#18788 = EDGE_CURVE ( 'NONE', #9128, #18103, #1367, .T. ) ;
#18789 = DIRECTION ( 'NONE',  ( -1.000000000000000000, -0.000000000000000000, -0.000000000000000000 ) ) ;
#18790 = CARTESIAN_POINT ( 'NONE',  ( 0.000000000000000000, 0.000000000000000000, 0.000000000000000000 ) ) ;
#18791 = CIRCLE ( 'NONE', #17874, 27.50000000000000000 ) ;
#18792 = LINE ( 'NONE', #2697, #18101 ) ;
#18793 = VERTEX_POINT ( 'NONE', #11736 ) ;
#18794 = CIRCLE ( 'NONE', #6011, 24.00000000002399858 ) ;
#18795 = CARTESIAN_POINT ( 'NONE',  ( -4.000000000000000000, 1.941961291383472732, -0.3515519931180205448 ) ) ;
#18796 = ORIENTED_EDGE ( 'NONE', *, *, #15041, .F. ) ;
#18797 = EDGE_CURVE ( 'NONE', #12056, #4178, #8335, .T. ) ;
#18798 = PRODUCT_DEFINITION_SHAPE ( 'NONE', 'NONE',  #18814 ) ;
#18799 = CARTESIAN_POINT ( 'NONE',  ( 0.000000000000000000, 0.000000000000000000, 0.000000000000000000 ) ) ;
#18800 = CARTESIAN_POINT ( 'NONE',  ( -90.00000000009001155, 2.081668171172168513E-14, -1.301042606982603940E-15 ) ) ;
#18801 = ORIENTED_EDGE ( 'NONE', *, *, #13325, .F. ) ;
#18802 = ORIENTED_EDGE ( 'NONE', *, *, #10109, .F. ) ;
#18803 = AXIS2_PLACEMENT_3D ( 'NONE', #14073, #6741, #852 ) ;
#18804 = AXIS2_PLACEMENT_3D ( 'NONE', #10884, #805, #16892 ) ;
#18805 = EDGE_CURVE ( 'NONE', #10656, #10272, #15939, .T. ) ;
#18806 = AXIS2_PLACEMENT_3D ( 'NONE', #11657, #14332, #1200 ) ;
#18807 = AXIS2_PLACEMENT_3D ( 'NONE', #17810, #10576, #9147 ) ;
#18808 = ORIENTED_EDGE ( 'NONE', *, *, #8215, .T. ) ;
#18809 = CARTESIAN_POINT ( 'NONE',  ( 10.00000000000000000, -44.70888270294186384, 34.13306034420170931 ) ) ;
#18810 = NEXT_ASSEMBLY_USAGE_OCCURRENCE ( 'NAUO1', ' ', ' ', #7121, #4673, $ ) ;
#18811 = NEXT_ASSEMBLY_USAGE_OCCURRENCE ( 'NAUO2', ' ', ' ', #7121, #8047, $ ) ;
#18812 = NEXT_ASSEMBLY_USAGE_OCCURRENCE ( 'NAUO3', ' ', ' ', #7121, #14453, $ ) ;
#18813 = NEXT_ASSEMBLY_USAGE_OCCURRENCE ( 'NAUO4', ' ', ' ', #7121, #8863, $ ) ;
#18814 = NEXT_ASSEMBLY_USAGE_OCCURRENCE ( 'NAUO5', ' ', ' ', #7121, #15382, $ ) ;
#18815 = NEXT_ASSEMBLY_USAGE_OCCURRENCE ( 'NAUO6', ' ', ' ', #7121, #1543, $ ) ;
#18816 = NEXT_ASSEMBLY_USAGE_OCCURRENCE ( 'NAUO7', ' ', ' ', #7121, #18768, $ ) ;
#18817 = NEXT_ASSEMBLY_USAGE_OCCURRENCE ( 'NAUO8', ' ', ' ', #7121, #8300, $ ) ;
#18818 = NEXT_ASSEMBLY_USAGE_OCCURRENCE ( 'NAUO9', ' ', ' ', #7121, #18184, $ ) ;
#18819 = NEXT_ASSEMBLY_USAGE_OCCURRENCE ( 'NAUO10', ' ', ' ', #7121, #15630, $ ) ;
#18820 = NEXT_ASSEMBLY_USAGE_OCCURRENCE ( 'NAUO11', ' ', ' ', #7121, #15630, $ ) ;
#18821 = NEXT_ASSEMBLY_USAGE_OCCURRENCE ( 'NAUO12', ' ', ' ', #7121, #15630, $ ) ;
#18822 = NEXT_ASSEMBLY_USAGE_OCCURRENCE ( 'NAUO13', ' ', ' ', #7121, #15630, $ ) ;
#18823 = NEXT_ASSEMBLY_USAGE_OCCURRENCE ( 'NAUO14', ' ', ' ', #7121, #15630, $ ) ;
#18824 = NEXT_ASSEMBLY_USAGE_OCCURRENCE ( 'NAUO15', ' ', ' ', #7121, #15630, $ ) ;
#18825 = NEXT_ASSEMBLY_USAGE_OCCURRENCE ( 'NAUO16', ' ', ' ', #7121, #15630, $ ) ;
#18826 = NEXT_ASSEMBLY_USAGE_OCCURRENCE ( 'NAUO17', ' ', ' ', #7121, #15630, $ ) ;
#18827 = NEXT_ASSEMBLY_USAGE_OCCURRENCE ( 'NAUO18', ' ', ' ', #7121, #15630, $ ) ;
#18828 = NEXT_ASSEMBLY_USAGE_OCCURRENCE ( 'NAUO19', ' ', ' ', #7121, #15630, $ ) ;
#18829 = NEXT_ASSEMBLY_USAGE_OCCURRENCE ( 'NAUO20', ' ', ' ', #7121, #13075, $ ) ;
#18830 = NEXT_ASSEMBLY_USAGE_OCCURRENCE ( 'NAUO21', ' ', ' ', #7121, #13075, $ ) ;
#18831 = NEXT_ASSEMBLY_USAGE_OCCURRENCE ( 'NAUO22', ' ', ' ', #7121, #13075, $ ) ;
#18832 = NEXT_ASSEMBLY_USAGE_OCCURRENCE ( 'NAUO23', ' ', ' ', #7121, #13075, $ ) ;
#18833 = NEXT_ASSEMBLY_USAGE_OCCURRENCE ( 'NAUO24', ' ', ' ', #7121, #13075, $ ) ;
#18834 = NEXT_ASSEMBLY_USAGE_OCCURRENCE ( 'NAUO25', ' ', ' ', #7121, #12243, $ ) ;
#18835 = NEXT_ASSEMBLY_USAGE_OCCURRENCE ( 'NAUO26', ' ', ' ', #7121, #12243, $ ) ;
#18836 = NEXT_ASSEMBLY_USAGE_OCCURRENCE ( 'NAUO27', ' ', ' ', #7121, #12243, $ ) ;
#18837 = NEXT_ASSEMBLY_USAGE_OCCURRENCE ( 'NAUO28', ' ', ' ', #7121, #12243, $ ) ;
#18838 = NEXT_ASSEMBLY_USAGE_OCCURRENCE ( 'NAUO29', ' ', ' ', #7121, #12243, $ ) ;
#18839 = NEXT_ASSEMBLY_USAGE_OCCURRENCE ( 'NAUO30', ' ', ' ', #7121, #12243, $ ) ;
#18840 = NEXT_ASSEMBLY_USAGE_OCCURRENCE ( 'NAUO31', ' ', ' ', #7121, #12243, $ ) ;
#18841 = NEXT_ASSEMBLY_USAGE_OCCURRENCE ( 'NAUO32', ' ', ' ', #7121, #12243, $ ) ;
#18842 = NEXT_ASSEMBLY_USAGE_OCCURRENCE ( 'NAUO33', ' ', ' ', #7121, #12243, $ ) ;
#18843 = NEXT_ASSEMBLY_USAGE_OCCURRENCE ( 'NAUO34', ' ', ' ', #7121, #12243, $ ) ;
#18844 = NEXT_ASSEMBLY_USAGE_OCCURRENCE ( 'NAUO35', ' ', ' ', #7121, #12243, $ ) ;
#18845 = NEXT_ASSEMBLY_USAGE_OCCURRENCE ( 'NAUO36', ' ', ' ', #7121, #12243, $ ) ;
#18846 = NEXT_ASSEMBLY_USAGE_OCCURRENCE ( 'NAUO37', ' ', ' ', #7121, #12243, $ ) ;
#18847 = NEXT_ASSEMBLY_USAGE_OCCURRENCE ( 'NAUO38', ' ', ' ', #7121, #12243, $ ) ;
#18848 = NEXT_ASSEMBLY_USAGE_OCCURRENCE ( 'NAUO39', ' ', ' ', #7121, #12243, $ ) ;
#18849=COLOUR_RGB('Dark Blue',0.08,0.2,0.34);
#18850=FILL_AREA_STYLE_COLOUR('',#18849);
#18851=FILL_AREA_STYLE('',(#18850));
#18852=SURFACE_STYLE_FILL_AREA(#18851);
#18853=SURFACE_SIDE_STYLE('',(#18852));
#18854=SURFACE_STYLE_USAGE(.BOTH.,#18853);
#18855=PRESENTATION_STYLE_ASSIGNMENT((#18854));
#18856=COLOUR_RGB('Light Blue',0.38,0.62,0.78);
#18857=FILL_AREA_STYLE_COLOUR('',#18856);
#18858=FILL_AREA_STYLE('',(#18857));
#18859=SURFACE_STYLE_FILL_AREA(#18858);
#18860=SURFACE_SIDE_STYLE('',(#18859));
#18861=SURFACE_STYLE_USAGE(.BOTH.,#18860);
#18862=PRESENTATION_STYLE_ASSIGNMENT((#18861));
#18863=COLOUR_RGB('Sky Blue',0.24,0.69,0.87);
#18864=FILL_AREA_STYLE_COLOUR('',#18863);
#18865=FILL_AREA_STYLE('',(#18864));
#18866=SURFACE_STYLE_FILL_AREA(#18865);
#18867=SURFACE_SIDE_STYLE('',(#18866));
#18868=SURFACE_STYLE_USAGE(.BOTH.,#18867);
#18869=PRESENTATION_STYLE_ASSIGNMENT((#18868));
#18870=COLOUR_RGB('Grey',0.48,0.52,0.57);
#18871=FILL_AREA_STYLE_COLOUR('',#18870);
#18872=FILL_AREA_STYLE('',(#18871));
#18873=SURFACE_STYLE_FILL_AREA(#18872);
#18874=SURFACE_SIDE_STYLE('',(#18873));
#18875=SURFACE_STYLE_USAGE(.BOTH.,#18874);
#18876=PRESENTATION_STYLE_ASSIGNMENT((#18875));
#18877=COLOUR_RGB('Black',0.12,0.14,0.17);
#18878=FILL_AREA_STYLE_COLOUR('',#18877);
#18879=FILL_AREA_STYLE('',(#18878));
#18880=SURFACE_STYLE_FILL_AREA(#18879);
#18881=SURFACE_SIDE_STYLE('',(#18880));
#18882=SURFACE_STYLE_USAGE(.BOTH.,#18881);
#18883=PRESENTATION_STYLE_ASSIGNMENT((#18882));
#18884=COLOUR_RGB('Off White',0.89,0.88,0.83);
#18885=FILL_AREA_STYLE_COLOUR('',#18884);
#18886=FILL_AREA_STYLE('',(#18885));
#18887=SURFACE_STYLE_FILL_AREA(#18886);
#18888=SURFACE_SIDE_STYLE('',(#18887));
#18889=SURFACE_STYLE_USAGE(.BOTH.,#18888);
#18890=PRESENTATION_STYLE_ASSIGNMENT((#18889));
ENDSEC;
END-ISO-10303-21;
